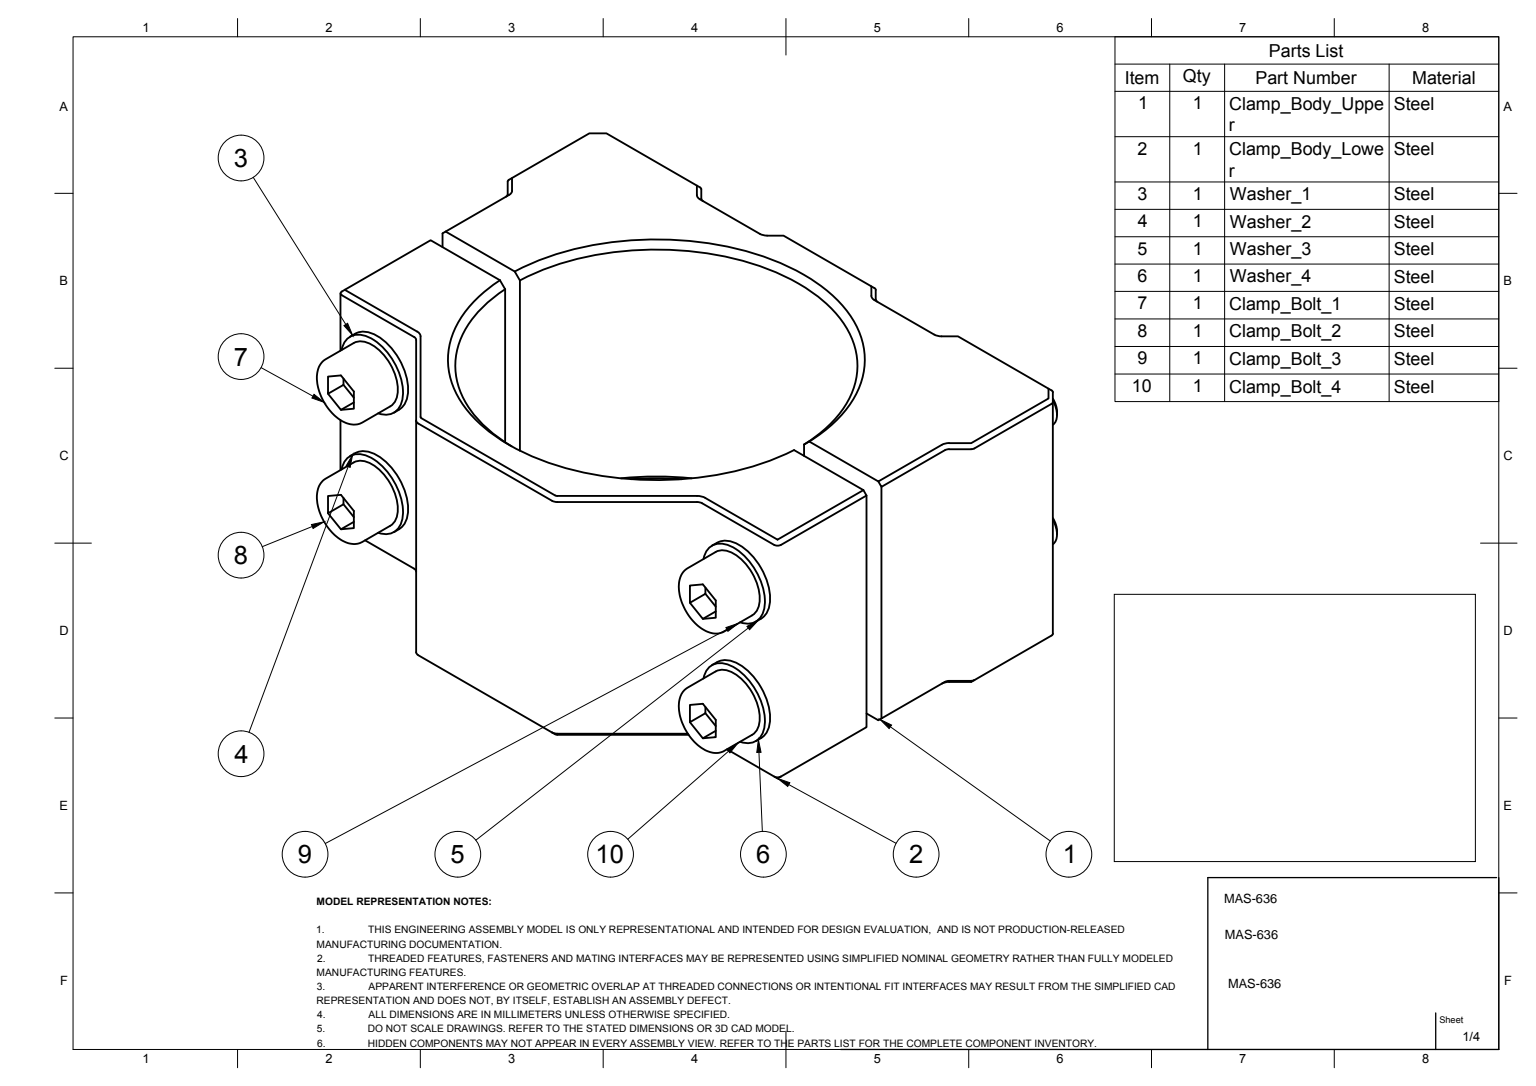
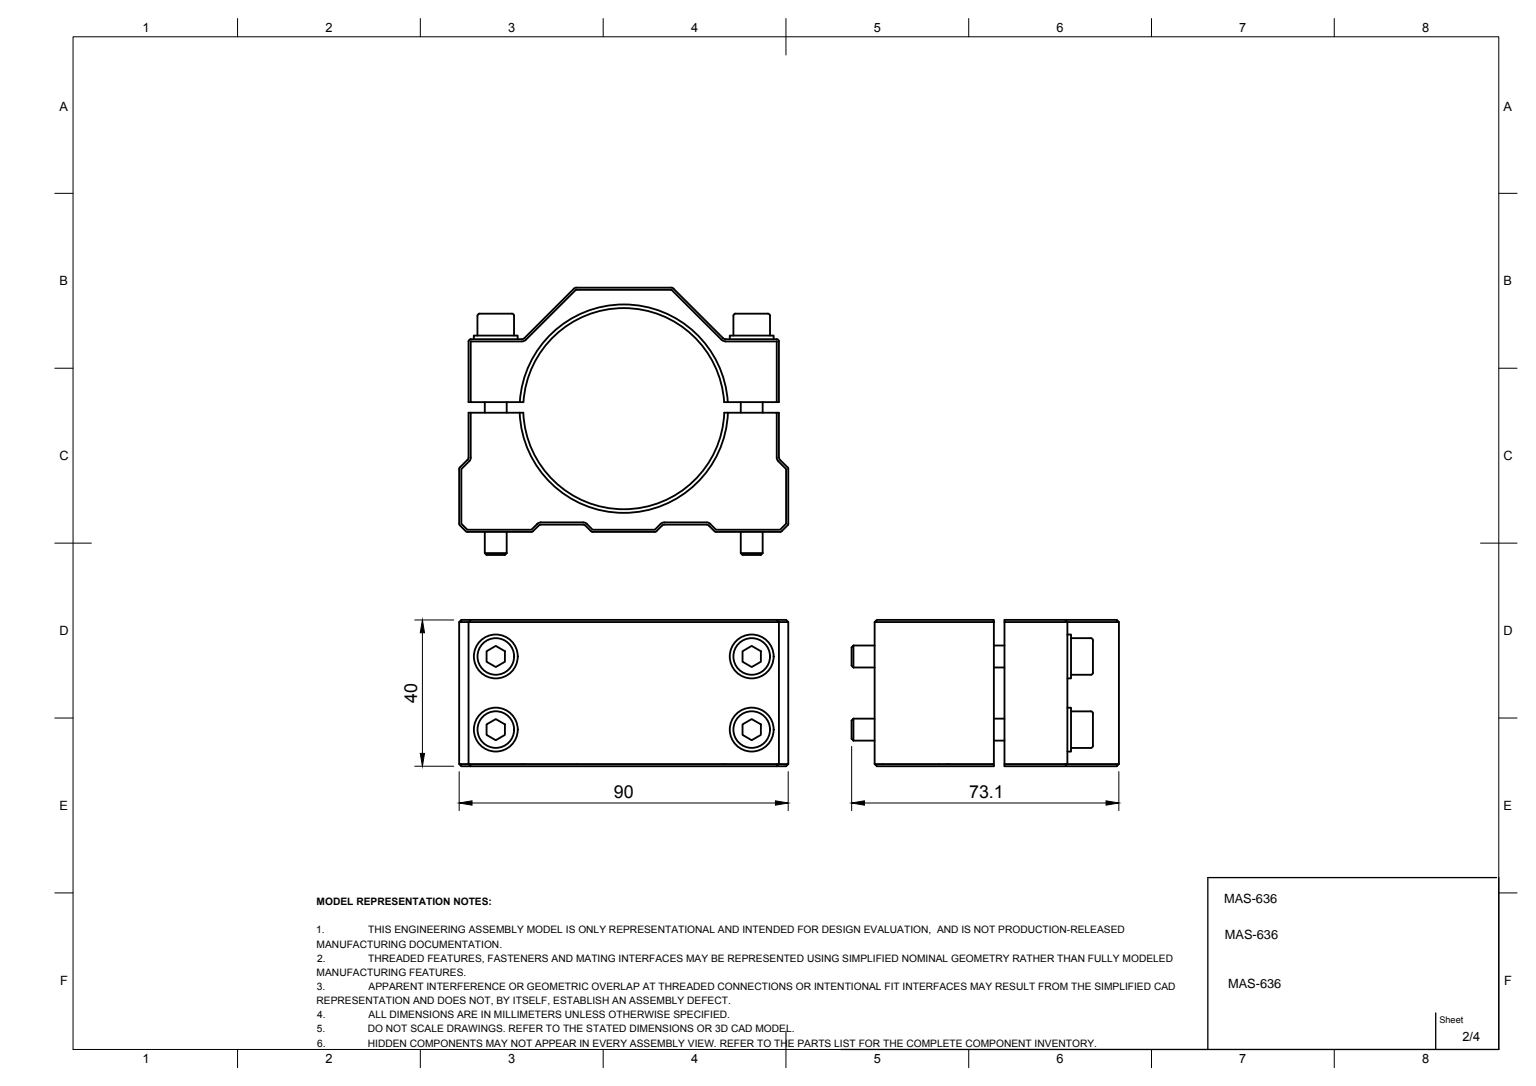
ISO-10303-21;
HEADER;
FILE_DESCRIPTION((''),'2;1');
FILE_NAME('MAS-636','2026-10-09T10:15:02-07:00',(''),(''),'','','');
FILE_SCHEMA (('AUTOMOTIVE_DESIGN { 1 0 10303 214 3 1 1 }'));
ENDSEC;
DATA;
#10 = MECHANICAL_DESIGN_GEOMETRIC_PRESENTATION_REPRESENTATION('',(#83,#84,
#85,#86,#87,#88,#89,#90,#91,#92),#6779) ;
#11 = ITEM_DEFINED_TRANSFORMATION($,$,#4017,#4427) ;
#12 = ITEM_DEFINED_TRANSFORMATION($,$,#4192,#4428) ;
#13 = ITEM_DEFINED_TRANSFORMATION($,$,#4291,#4429) ;
#14 = ITEM_DEFINED_TRANSFORMATION($,$,#4300,#4430) ;
#15 = ITEM_DEFINED_TRANSFORMATION($,$,#4309,#4431) ;
#16 = ITEM_DEFINED_TRANSFORMATION($,$,#4318,#4432) ;
#17 = ITEM_DEFINED_TRANSFORMATION($,$,#4327,#4433) ;
#18 = ITEM_DEFINED_TRANSFORMATION($,$,#4352,#4434) ;
#19 = ITEM_DEFINED_TRANSFORMATION($,$,#4377,#4435) ;
#20 = ITEM_DEFINED_TRANSFORMATION($,$,#4402,#4436) ;
#21 = (
REPRESENTATION_RELATIONSHIP($,$,#6817,#6816)
REPRESENTATION_RELATIONSHIP_WITH_TRANSFORMATION(#11)
SHAPE_REPRESENTATION_RELATIONSHIP()
) ;
#22 = (
REPRESENTATION_RELATIONSHIP($,$,#6818,#6816)
REPRESENTATION_RELATIONSHIP_WITH_TRANSFORMATION(#12)
SHAPE_REPRESENTATION_RELATIONSHIP()
) ;
#23 = (
REPRESENTATION_RELATIONSHIP($,$,#6819,#6816)
REPRESENTATION_RELATIONSHIP_WITH_TRANSFORMATION(#13)
SHAPE_REPRESENTATION_RELATIONSHIP()
) ;
#24 = (
REPRESENTATION_RELATIONSHIP($,$,#6820,#6816)
REPRESENTATION_RELATIONSHIP_WITH_TRANSFORMATION(#14)
SHAPE_REPRESENTATION_RELATIONSHIP()
) ;
#25 = (
REPRESENTATION_RELATIONSHIP($,$,#6821,#6816)
REPRESENTATION_RELATIONSHIP_WITH_TRANSFORMATION(#15)
SHAPE_REPRESENTATION_RELATIONSHIP()
) ;
#26 = (
REPRESENTATION_RELATIONSHIP($,$,#6822,#6816)
REPRESENTATION_RELATIONSHIP_WITH_TRANSFORMATION(#16)
SHAPE_REPRESENTATION_RELATIONSHIP()
) ;
#27 = (
REPRESENTATION_RELATIONSHIP($,$,#6823,#6816)
REPRESENTATION_RELATIONSHIP_WITH_TRANSFORMATION(#17)
SHAPE_REPRESENTATION_RELATIONSHIP()
) ;
#28 = (
REPRESENTATION_RELATIONSHIP($,$,#6824,#6816)
REPRESENTATION_RELATIONSHIP_WITH_TRANSFORMATION(#18)
SHAPE_REPRESENTATION_RELATIONSHIP()
) ;
#29 = (
REPRESENTATION_RELATIONSHIP($,$,#6825,#6816)
REPRESENTATION_RELATIONSHIP_WITH_TRANSFORMATION(#19)
SHAPE_REPRESENTATION_RELATIONSHIP()
) ;
#30 = (
REPRESENTATION_RELATIONSHIP($,$,#6826,#6816)
REPRESENTATION_RELATIONSHIP_WITH_TRANSFORMATION(#20)
SHAPE_REPRESENTATION_RELATIONSHIP()
) ;
#31 = CONTEXT_DEPENDENT_SHAPE_REPRESENTATION(#21,#6806) ;
#32 = CONTEXT_DEPENDENT_SHAPE_REPRESENTATION(#22,#6807) ;
#33 = CONTEXT_DEPENDENT_SHAPE_REPRESENTATION(#23,#6808) ;
#34 = CONTEXT_DEPENDENT_SHAPE_REPRESENTATION(#24,#6809) ;
#35 = CONTEXT_DEPENDENT_SHAPE_REPRESENTATION(#25,#6810) ;
#36 = CONTEXT_DEPENDENT_SHAPE_REPRESENTATION(#26,#6811) ;
#37 = CONTEXT_DEPENDENT_SHAPE_REPRESENTATION(#27,#6812) ;
#38 = CONTEXT_DEPENDENT_SHAPE_REPRESENTATION(#28,#6813) ;
#39 = CONTEXT_DEPENDENT_SHAPE_REPRESENTATION(#29,#6814) ;
#40 = CONTEXT_DEPENDENT_SHAPE_REPRESENTATION(#30,#6815) ;
#41 = NEXT_ASSEMBLY_USAGE_OCCURRENCE('Clamp_Body_Upper:1',
'Clamp_Body_Upper:1','Clamp_Body_Upper:1',#6828,#6829,
'Clamp_Body_Upper:1') ;
#42 = NEXT_ASSEMBLY_USAGE_OCCURRENCE('Clamp_Body_Lower:1',
'Clamp_Body_Lower:1','Clamp_Body_Lower:1',#6828,#6830,
'Clamp_Body_Lower:1') ;
#43 = NEXT_ASSEMBLY_USAGE_OCCURRENCE('Washer_1:1','Washer_1:1',
'Washer_1:1',#6828,#6831,'Washer_1:1') ;
#44 = NEXT_ASSEMBLY_USAGE_OCCURRENCE('Washer_2:1','Washer_2:1',
'Washer_2:1',#6828,#6832,'Washer_2:1') ;
#45 = NEXT_ASSEMBLY_USAGE_OCCURRENCE('Washer_3:1','Washer_3:1',
'Washer_3:1',#6828,#6833,'Washer_3:1') ;
#46 = NEXT_ASSEMBLY_USAGE_OCCURRENCE('Washer_4:1','Washer_4:1',
'Washer_4:1',#6828,#6834,'Washer_4:1') ;
#47 = NEXT_ASSEMBLY_USAGE_OCCURRENCE('Clamp_Bolt_1:1','Clamp_Bolt_1:1',
'Clamp_Bolt_1:1',#6828,#6835,'Clamp_Bolt_1:1') ;
#48 = NEXT_ASSEMBLY_USAGE_OCCURRENCE('Clamp_Bolt_2:1','Clamp_Bolt_2:1',
'Clamp_Bolt_2:1',#6828,#6836,'Clamp_Bolt_2:1') ;
#49 = NEXT_ASSEMBLY_USAGE_OCCURRENCE('Clamp_Bolt_3:1','Clamp_Bolt_3:1',
'Clamp_Bolt_3:1',#6828,#6837,'Clamp_Bolt_3:1') ;
#50 = NEXT_ASSEMBLY_USAGE_OCCURRENCE('Clamp_Bolt_4:1','Clamp_Bolt_4:1',
'Clamp_Bolt_4:1',#6828,#6838,'Clamp_Bolt_4:1') ;
#51 = TOROIDAL_SURFACE('',#4342,4.4,0.6) ;
#52 = TOROIDAL_SURFACE('',#4346,3.25,0.25) ;
#53 = TOROIDAL_SURFACE('',#4367,4.4,0.6) ;
#54 = TOROIDAL_SURFACE('',#4371,3.25,0.25) ;
#55 = TOROIDAL_SURFACE('',#4392,4.4,0.6) ;
#56 = TOROIDAL_SURFACE('',#4396,3.25,0.25) ;
#57 = TOROIDAL_SURFACE('',#4417,4.4,0.6) ;
#58 = TOROIDAL_SURFACE('',#4421,3.25,0.25) ;
#59 = B_SPLINE_CURVE_WITH_KNOTS('',3,(#6151,#6152,#6153,#6154),
 .UNSPECIFIED.,.F.,.F.,(4,4),(0.,2.0142284459),.UNSPECIFIED.) ;
#60 = B_SPLINE_CURVE_WITH_KNOTS('',3,(#6158,#6159,#6160,#6161),
 .UNSPECIFIED.,.F.,.F.,(4,4),(0.,2.0142284459),.UNSPECIFIED.) ;
#61 = B_SPLINE_CURVE_WITH_KNOTS('',3,(#6173,#6174,#6175,#6176),
 .UNSPECIFIED.,.F.,.F.,(4,4),(0.,2.0142284459),.UNSPECIFIED.) ;
#62 = B_SPLINE_CURVE_WITH_KNOTS('',3,(#6177,#6178,#6179,#6180),
 .UNSPECIFIED.,.F.,.F.,(4,4),(0.,2.0142284459),.UNSPECIFIED.) ;
#63 = SHAPE_REPRESENTATION_RELATIONSHIP('SRR','None',#6817,#73) ;
#64 = SHAPE_REPRESENTATION_RELATIONSHIP('SRR','None',#6818,#74) ;
#65 = SHAPE_REPRESENTATION_RELATIONSHIP('SRR','None',#6819,#75) ;
#66 = SHAPE_REPRESENTATION_RELATIONSHIP('SRR','None',#6820,#76) ;
#67 = SHAPE_REPRESENTATION_RELATIONSHIP('SRR','None',#6821,#77) ;
#68 = SHAPE_REPRESENTATION_RELATIONSHIP('SRR','None',#6822,#78) ;
#69 = SHAPE_REPRESENTATION_RELATIONSHIP('SRR','None',#6823,#79) ;
#70 = SHAPE_REPRESENTATION_RELATIONSHIP('SRR','None',#6824,#80) ;
#71 = SHAPE_REPRESENTATION_RELATIONSHIP('SRR','None',#6825,#81) ;
#72 = SHAPE_REPRESENTATION_RELATIONSHIP('SRR','None',#6826,#82) ;
#73 = ADVANCED_BREP_SHAPE_REPRESENTATION('',(#93),#6769) ;
#74 = ADVANCED_BREP_SHAPE_REPRESENTATION('',(#94),#6770) ;
#75 = ADVANCED_BREP_SHAPE_REPRESENTATION('',(#95),#6771) ;
#76 = ADVANCED_BREP_SHAPE_REPRESENTATION('',(#96),#6772) ;
#77 = ADVANCED_BREP_SHAPE_REPRESENTATION('',(#97),#6773) ;
#78 = ADVANCED_BREP_SHAPE_REPRESENTATION('',(#98),#6774) ;
#79 = ADVANCED_BREP_SHAPE_REPRESENTATION('',(#99),#6775) ;
#80 = ADVANCED_BREP_SHAPE_REPRESENTATION('',(#100),#6776) ;
#81 = ADVANCED_BREP_SHAPE_REPRESENTATION('',(#101),#6777) ;
#82 = ADVANCED_BREP_SHAPE_REPRESENTATION('',(#102),#6778) ;
#83 = STYLED_ITEM('',(#6876),#93) ;
#84 = STYLED_ITEM('',(#6876),#94) ;
#85 = STYLED_ITEM('',(#6877),#95) ;
#86 = STYLED_ITEM('',(#6877),#96) ;
#87 = STYLED_ITEM('',(#6877),#97) ;
#88 = STYLED_ITEM('',(#6877),#98) ;
#89 = STYLED_ITEM('',(#6877),#99) ;
#90 = STYLED_ITEM('',(#6877),#100) ;
#91 = STYLED_ITEM('',(#6877),#101) ;
#92 = STYLED_ITEM('',(#6877),#102) ;
#93 = MANIFOLD_SOLID_BREP('Body1',#3895) ;
#94 = MANIFOLD_SOLID_BREP('Body1',#3896) ;
#95 = MANIFOLD_SOLID_BREP('Body1',#3897) ;
#96 = MANIFOLD_SOLID_BREP('Body1',#3898) ;
#97 = MANIFOLD_SOLID_BREP('Body1',#3899) ;
#98 = MANIFOLD_SOLID_BREP('Body1',#3900) ;
#99 = MANIFOLD_SOLID_BREP('Body1',#3901) ;
#100 = MANIFOLD_SOLID_BREP('Body1',#3902) ;
#101 = MANIFOLD_SOLID_BREP('Body1',#3903) ;
#102 = MANIFOLD_SOLID_BREP('Body1',#3904) ;
#103 = FACE_BOUND('',#628,.T.) ;
#104 = FACE_BOUND('',#629,.T.) ;
#105 = FACE_BOUND('',#631,.T.) ;
#106 = FACE_BOUND('',#632,.T.) ;
#107 = FACE_BOUND('',#638,.T.) ;
#108 = FACE_BOUND('',#639,.T.) ;
#109 = FACE_BOUND('',#649,.T.) ;
#110 = FACE_BOUND('',#650,.T.) ;
#111 = FACE_BOUND('',#719,.T.) ;
#112 = FACE_BOUND('',#720,.T.) ;
#113 = FACE_BOUND('',#722,.T.) ;
#114 = FACE_BOUND('',#723,.T.) ;
#115 = FACE_BOUND('',#745,.T.) ;
#116 = FACE_BOUND('',#746,.T.) ;
#117 = FACE_BOUND('',#752,.T.) ;
#118 = FACE_BOUND('',#753,.T.) ;
#119 = FACE_BOUND('',#758,.T.) ;
#120 = FACE_BOUND('',#760,.T.) ;
#121 = FACE_BOUND('',#764,.T.) ;
#122 = FACE_BOUND('',#766,.T.) ;
#123 = FACE_BOUND('',#770,.T.) ;
#124 = FACE_BOUND('',#772,.T.) ;
#125 = FACE_BOUND('',#776,.T.) ;
#126 = FACE_BOUND('',#778,.T.) ;
#127 = FACE_BOUND('',#787,.T.) ;
#128 = FACE_BOUND('',#789,.T.) ;
#129 = FACE_BOUND('',#804,.T.) ;
#130 = FACE_BOUND('',#806,.T.) ;
#131 = FACE_BOUND('',#821,.T.) ;
#132 = FACE_BOUND('',#823,.T.) ;
#133 = FACE_BOUND('',#838,.T.) ;
#134 = FACE_BOUND('',#840,.T.) ;
#135 = PLANE('',#4045) ;
#136 = PLANE('',#4054) ;
#137 = PLANE('',#4057) ;
#138 = PLANE('',#4060) ;
#139 = PLANE('',#4063) ;
#140 = PLANE('',#4066) ;
#141 = PLANE('',#4069) ;
#142 = PLANE('',#4072) ;
#143 = PLANE('',#4075) ;
#144 = PLANE('',#4078) ;
#145 = PLANE('',#4081) ;
#146 = PLANE('',#4084) ;
#147 = PLANE('',#4087) ;
#148 = PLANE('',#4090) ;
#149 = PLANE('',#4093) ;
#150 = PLANE('',#4096) ;
#151 = PLANE('',#4099) ;
#152 = PLANE('',#4100) ;
#153 = PLANE('',#4101) ;
#154 = PLANE('',#4120) ;
#155 = PLANE('',#4121) ;
#156 = PLANE('',#4122) ;
#157 = PLANE('',#4123) ;
#158 = PLANE('',#4124) ;
#159 = PLANE('',#4125) ;
#160 = PLANE('',#4128) ;
#161 = PLANE('',#4131) ;
#162 = PLANE('',#4132) ;
#163 = PLANE('',#4135) ;
#164 = PLANE('',#4138) ;
#165 = PLANE('',#4139) ;
#166 = PLANE('',#4142) ;
#167 = PLANE('',#4145) ;
#168 = PLANE('',#4148) ;
#169 = PLANE('',#4151) ;
#170 = PLANE('',#4152) ;
#171 = PLANE('',#4155) ;
#172 = PLANE('',#4156) ;
#173 = PLANE('',#4160) ;
#174 = PLANE('',#4162) ;
#175 = PLANE('',#4164) ;
#176 = PLANE('',#4166) ;
#177 = PLANE('',#4168) ;
#178 = PLANE('',#4170) ;
#179 = PLANE('',#4172) ;
#180 = PLANE('',#4174) ;
#181 = PLANE('',#4176) ;
#182 = PLANE('',#4178) ;
#183 = PLANE('',#4180) ;
#184 = PLANE('',#4182) ;
#185 = PLANE('',#4184) ;
#186 = PLANE('',#4186) ;
#187 = PLANE('',#4188) ;
#188 = PLANE('',#4190) ;
#189 = PLANE('',#4191) ;
#190 = PLANE('',#4200) ;
#191 = PLANE('',#4209) ;
#192 = PLANE('',#4212) ;
#193 = PLANE('',#4215) ;
#194 = PLANE('',#4218) ;
#195 = PLANE('',#4221) ;
#196 = PLANE('',#4224) ;
#197 = PLANE('',#4225) ;
#198 = PLANE('',#4226) ;
#199 = PLANE('',#4237) ;
#200 = PLANE('',#4238) ;
#201 = PLANE('',#4241) ;
#202 = PLANE('',#4244) ;
#203 = PLANE('',#4247) ;
#204 = PLANE('',#4250) ;
#205 = PLANE('',#4253) ;
#206 = PLANE('',#4257) ;
#207 = PLANE('',#4259) ;
#208 = PLANE('',#4261) ;
#209 = PLANE('',#4263) ;
#210 = PLANE('',#4265) ;
#211 = PLANE('',#4267) ;
#212 = PLANE('',#4268) ;
#213 = PLANE('',#4277) ;
#214 = PLANE('',#4288) ;
#215 = PLANE('',#4298) ;
#216 = PLANE('',#4299) ;
#217 = PLANE('',#4307) ;
#218 = PLANE('',#4308) ;
#219 = PLANE('',#4316) ;
#220 = PLANE('',#4317) ;
#221 = PLANE('',#4325) ;
#222 = PLANE('',#4326) ;
#223 = PLANE('',#4328) ;
#224 = PLANE('',#4329) ;
#225 = PLANE('',#4330) ;
#226 = PLANE('',#4331) ;
#227 = PLANE('',#4332) ;
#228 = PLANE('',#4333) ;
#229 = PLANE('',#4334) ;
#230 = PLANE('',#4335) ;
#231 = PLANE('',#4337) ;
#232 = PLANE('',#4340) ;
#233 = PLANE('',#4353) ;
#234 = PLANE('',#4354) ;
#235 = PLANE('',#4355) ;
#236 = PLANE('',#4356) ;
#237 = PLANE('',#4357) ;
#238 = PLANE('',#4358) ;
#239 = PLANE('',#4359) ;
#240 = PLANE('',#4360) ;
#241 = PLANE('',#4362) ;
#242 = PLANE('',#4365) ;
#243 = PLANE('',#4378) ;
#244 = PLANE('',#4379) ;
#245 = PLANE('',#4380) ;
#246 = PLANE('',#4381) ;
#247 = PLANE('',#4382) ;
#248 = PLANE('',#4383) ;
#249 = PLANE('',#4384) ;
#250 = PLANE('',#4385) ;
#251 = PLANE('',#4387) ;
#252 = PLANE('',#4390) ;
#253 = PLANE('',#4403) ;
#254 = PLANE('',#4404) ;
#255 = PLANE('',#4405) ;
#256 = PLANE('',#4406) ;
#257 = PLANE('',#4407) ;
#258 = PLANE('',#4408) ;
#259 = PLANE('',#4409) ;
#260 = PLANE('',#4410) ;
#261 = PLANE('',#4412) ;
#262 = PLANE('',#4415) ;
#263 = (
BOUNDED_CURVE()
B_SPLINE_CURVE(2,(#5652,#5653,#5654),.UNSPECIFIED.,.F.,.F.)
B_SPLINE_CURVE_WITH_KNOTS((3,3),(8.17571637705571,8.18145882895963),
 .UNSPECIFIED.)
CURVE()
GEOMETRIC_REPRESENTATION_ITEM()
RATIONAL_B_SPLINE_CURVE((1.06993006993377,1.0518696293833,1.03378378378363))
REPRESENTATION_ITEM('')
) ;
#264 = (
BOUNDED_CURVE()
B_SPLINE_CURVE(2,(#5656,#5657,#5658),.UNSPECIFIED.,.F.,.F.)
B_SPLINE_CURVE_WITH_KNOTS((3,3),(-0.0111022969227764,-0.00535984501964869),
 .UNSPECIFIED.)
CURVE()
GEOMETRIC_REPRESENTATION_ITEM()
RATIONAL_B_SPLINE_CURVE((1.06993006993377,1.0518696293858,1.03378378378863))
REPRESENTATION_ITEM('')
) ;
#265 = (
BOUNDED_CURVE()
B_SPLINE_CURVE(2,(#5664,#5665,#5666),.UNSPECIFIED.,.F.,.F.)
B_SPLINE_CURVE_WITH_KNOTS((3,3),(8.1757163770557,8.18145882895962),
 .UNSPECIFIED.)
CURVE()
GEOMETRIC_REPRESENTATION_ITEM()
RATIONAL_B_SPLINE_CURVE((1.06993006993376,1.05186962938329,1.03378378378362))
REPRESENTATION_ITEM('')
) ;
#266 = (
BOUNDED_CURVE()
B_SPLINE_CURVE(2,(#5667,#5668,#5669),.UNSPECIFIED.,.F.,.F.)
B_SPLINE_CURVE_WITH_KNOTS((3,3),(-0.0111022969227769,-0.00535984501964911),
 .UNSPECIFIED.)
CURVE()
GEOMETRIC_REPRESENTATION_ITEM()
RATIONAL_B_SPLINE_CURVE((1.06993006993377,1.0518696293858,1.03378378378863))
REPRESENTATION_ITEM('')
) ;
#267 = CONICAL_SURFACE('',#4021,1.,0.785398163397) ;
#268 = CONICAL_SURFACE('',#4023,1.,0.785398163397) ;
#269 = CONICAL_SURFACE('',#4028,1.,0.785398163398) ;
#270 = CONICAL_SURFACE('',#4033,1.,0.785398163398) ;
#271 = CONICAL_SURFACE('',#4038,1.,0.785398163398) ;
#272 = CONICAL_SURFACE('',#4043,1.,0.785398163398) ;
#273 = CONICAL_SURFACE('',#4052,1.,0.785398163392) ;
#274 = CONICAL_SURFACE('',#4055,1.,0.785398163397) ;
#275 = CONICAL_SURFACE('',#4058,1.,0.785398163397) ;
#276 = CONICAL_SURFACE('',#4061,1.,0.785398163397) ;
#277 = CONICAL_SURFACE('',#4064,1.,0.785398163397) ;
#278 = CONICAL_SURFACE('',#4067,1.,0.785398163392) ;
#279 = CONICAL_SURFACE('',#4070,1.,0.785398163392) ;
#280 = CONICAL_SURFACE('',#4073,1.,0.785398163397) ;
#281 = CONICAL_SURFACE('',#4076,1.,0.785398163397) ;
#282 = CONICAL_SURFACE('',#4079,1.,0.785398163397) ;
#283 = CONICAL_SURFACE('',#4082,1.,0.785398163397) ;
#284 = CONICAL_SURFACE('',#4085,1.,0.785398163397) ;
#285 = CONICAL_SURFACE('',#4088,1.,0.785398163397) ;
#286 = CONICAL_SURFACE('',#4091,1.,0.785398163397) ;
#287 = CONICAL_SURFACE('',#4094,1.,0.785398163397) ;
#288 = CONICAL_SURFACE('',#4097,1.,0.785398163397) ;
#289 = CONICAL_SURFACE('',#4159,1.,0.785398163392) ;
#290 = CONICAL_SURFACE('',#4161,1.,0.785398163397) ;
#291 = CONICAL_SURFACE('',#4163,1.,0.785398163397) ;
#292 = CONICAL_SURFACE('',#4165,1.,0.785398163397) ;
#293 = CONICAL_SURFACE('',#4167,1.,0.785398163397) ;
#294 = CONICAL_SURFACE('',#4169,1.,0.785398163372) ;
#295 = CONICAL_SURFACE('',#4171,1.,0.785398163372) ;
#296 = CONICAL_SURFACE('',#4173,1.,0.785398163397) ;
#297 = CONICAL_SURFACE('',#4175,1.,0.785398163397) ;
#298 = CONICAL_SURFACE('',#4177,1.,0.785398163397) ;
#299 = CONICAL_SURFACE('',#4179,1.,0.785398163397) ;
#300 = CONICAL_SURFACE('',#4181,1.,0.785398163397) ;
#301 = CONICAL_SURFACE('',#4183,1.,0.785398163397) ;
#302 = CONICAL_SURFACE('',#4185,1.,0.785398163397) ;
#303 = CONICAL_SURFACE('',#4187,1.,0.785398163397) ;
#304 = CONICAL_SURFACE('',#4189,1.,0.785398163397) ;
#305 = CONICAL_SURFACE('',#4193,1.,0.785398163397) ;
#306 = CONICAL_SURFACE('',#4198,1.,0.785398163397) ;
#307 = CONICAL_SURFACE('',#4207,1.,0.785398163397) ;
#308 = CONICAL_SURFACE('',#4210,1.,0.785398163397) ;
#309 = CONICAL_SURFACE('',#4213,1.,0.785398163397) ;
#310 = CONICAL_SURFACE('',#4216,1.,0.785398163397) ;
#311 = CONICAL_SURFACE('',#4219,1.,0.785398163397) ;
#312 = CONICAL_SURFACE('',#4222,1.,0.785398163397) ;
#313 = CONICAL_SURFACE('',#4256,1.,0.785398163397) ;
#314 = CONICAL_SURFACE('',#4258,1.,0.785398163397) ;
#315 = CONICAL_SURFACE('',#4260,1.,0.785398163397) ;
#316 = CONICAL_SURFACE('',#4262,1.,0.785398163397) ;
#317 = CONICAL_SURFACE('',#4264,1.,0.785398163397) ;
#318 = CONICAL_SURFACE('',#4266,1.,0.785398163397) ;
#319 = CONICAL_SURFACE('',#4272,1.,0.785398163398) ;
#320 = CONICAL_SURFACE('',#4279,1.,0.785398163398) ;
#321 = CONICAL_SURFACE('',#4283,1.,0.785398163398) ;
#322 = CONICAL_SURFACE('',#4290,1.,0.785398163398) ;
#323 = CONICAL_SURFACE('',#4351,2.5,0.785398163397) ;
#324 = CONICAL_SURFACE('',#4376,2.5,0.785398163397) ;
#325 = CONICAL_SURFACE('',#4401,2.5,0.785398163397) ;
#326 = CONICAL_SURFACE('',#4426,2.5,0.785398163397) ;
#327 = FACE_OUTER_BOUND('',#571,.T.) ;
#328 = FACE_OUTER_BOUND('',#572,.T.) ;
#329 = FACE_OUTER_BOUND('',#573,.T.) ;
#330 = FACE_OUTER_BOUND('',#574,.T.) ;
#331 = FACE_OUTER_BOUND('',#575,.T.) ;
#332 = FACE_OUTER_BOUND('',#576,.T.) ;
#333 = FACE_OUTER_BOUND('',#577,.T.) ;
#334 = FACE_OUTER_BOUND('',#578,.T.) ;
#335 = FACE_OUTER_BOUND('',#579,.T.) ;
#336 = FACE_OUTER_BOUND('',#580,.T.) ;
#337 = FACE_OUTER_BOUND('',#581,.T.) ;
#338 = FACE_OUTER_BOUND('',#582,.T.) ;
#339 = FACE_OUTER_BOUND('',#583,.T.) ;
#340 = FACE_OUTER_BOUND('',#584,.T.) ;
#341 = FACE_OUTER_BOUND('',#585,.T.) ;
#342 = FACE_OUTER_BOUND('',#586,.T.) ;
#343 = FACE_OUTER_BOUND('',#587,.T.) ;
#344 = FACE_OUTER_BOUND('',#588,.T.) ;
#345 = FACE_OUTER_BOUND('',#589,.T.) ;
#346 = FACE_OUTER_BOUND('',#590,.T.) ;
#347 = FACE_OUTER_BOUND('',#591,.T.) ;
#348 = FACE_OUTER_BOUND('',#592,.T.) ;
#349 = FACE_OUTER_BOUND('',#593,.T.) ;
#350 = FACE_OUTER_BOUND('',#594,.T.) ;
#351 = FACE_OUTER_BOUND('',#595,.T.) ;
#352 = FACE_OUTER_BOUND('',#596,.T.) ;
#353 = FACE_OUTER_BOUND('',#597,.T.) ;
#354 = FACE_OUTER_BOUND('',#598,.T.) ;
#355 = FACE_OUTER_BOUND('',#599,.T.) ;
#356 = FACE_OUTER_BOUND('',#600,.T.) ;
#357 = FACE_OUTER_BOUND('',#601,.T.) ;
#358 = FACE_OUTER_BOUND('',#602,.T.) ;
#359 = FACE_OUTER_BOUND('',#603,.T.) ;
#360 = FACE_OUTER_BOUND('',#604,.T.) ;
#361 = FACE_OUTER_BOUND('',#605,.T.) ;
#362 = FACE_OUTER_BOUND('',#606,.T.) ;
#363 = FACE_OUTER_BOUND('',#607,.T.) ;
#364 = FACE_OUTER_BOUND('',#608,.T.) ;
#365 = FACE_OUTER_BOUND('',#609,.T.) ;
#366 = FACE_OUTER_BOUND('',#610,.T.) ;
#367 = FACE_OUTER_BOUND('',#611,.T.) ;
#368 = FACE_OUTER_BOUND('',#612,.T.) ;
#369 = FACE_OUTER_BOUND('',#613,.T.) ;
#370 = FACE_OUTER_BOUND('',#614,.T.) ;
#371 = FACE_OUTER_BOUND('',#615,.T.) ;
#372 = FACE_OUTER_BOUND('',#616,.T.) ;
#373 = FACE_OUTER_BOUND('',#617,.T.) ;
#374 = FACE_OUTER_BOUND('',#618,.T.) ;
#375 = FACE_OUTER_BOUND('',#619,.T.) ;
#376 = FACE_OUTER_BOUND('',#620,.T.) ;
#377 = FACE_OUTER_BOUND('',#621,.T.) ;
#378 = FACE_OUTER_BOUND('',#622,.T.) ;
#379 = FACE_OUTER_BOUND('',#623,.T.) ;
#380 = FACE_OUTER_BOUND('',#624,.T.) ;
#381 = FACE_OUTER_BOUND('',#625,.T.) ;
#382 = FACE_OUTER_BOUND('',#626,.T.) ;
#383 = FACE_OUTER_BOUND('',#627,.T.) ;
#384 = FACE_OUTER_BOUND('',#630,.T.) ;
#385 = FACE_OUTER_BOUND('',#633,.T.) ;
#386 = FACE_OUTER_BOUND('',#634,.T.) ;
#387 = FACE_OUTER_BOUND('',#635,.T.) ;
#388 = FACE_OUTER_BOUND('',#636,.T.) ;
#389 = FACE_OUTER_BOUND('',#637,.T.) ;
#390 = FACE_OUTER_BOUND('',#640,.T.) ;
#391 = FACE_OUTER_BOUND('',#641,.T.) ;
#392 = FACE_OUTER_BOUND('',#642,.T.) ;
#393 = FACE_OUTER_BOUND('',#643,.T.) ;
#394 = FACE_OUTER_BOUND('',#644,.T.) ;
#395 = FACE_OUTER_BOUND('',#645,.T.) ;
#396 = FACE_OUTER_BOUND('',#646,.T.) ;
#397 = FACE_OUTER_BOUND('',#647,.T.) ;
#398 = FACE_OUTER_BOUND('',#648,.T.) ;
#399 = FACE_OUTER_BOUND('',#651,.T.) ;
#400 = FACE_OUTER_BOUND('',#652,.T.) ;
#401 = FACE_OUTER_BOUND('',#653,.T.) ;
#402 = FACE_OUTER_BOUND('',#654,.T.) ;
#403 = FACE_OUTER_BOUND('',#655,.T.) ;
#404 = FACE_OUTER_BOUND('',#656,.T.) ;
#405 = FACE_OUTER_BOUND('',#657,.T.) ;
#406 = FACE_OUTER_BOUND('',#658,.T.) ;
#407 = FACE_OUTER_BOUND('',#659,.T.) ;
#408 = FACE_OUTER_BOUND('',#660,.T.) ;
#409 = FACE_OUTER_BOUND('',#661,.T.) ;
#410 = FACE_OUTER_BOUND('',#662,.T.) ;
#411 = FACE_OUTER_BOUND('',#663,.T.) ;
#412 = FACE_OUTER_BOUND('',#664,.T.) ;
#413 = FACE_OUTER_BOUND('',#665,.T.) ;
#414 = FACE_OUTER_BOUND('',#666,.T.) ;
#415 = FACE_OUTER_BOUND('',#667,.T.) ;
#416 = FACE_OUTER_BOUND('',#668,.T.) ;
#417 = FACE_OUTER_BOUND('',#669,.T.) ;
#418 = FACE_OUTER_BOUND('',#670,.T.) ;
#419 = FACE_OUTER_BOUND('',#671,.T.) ;
#420 = FACE_OUTER_BOUND('',#672,.T.) ;
#421 = FACE_OUTER_BOUND('',#673,.T.) ;
#422 = FACE_OUTER_BOUND('',#674,.T.) ;
#423 = FACE_OUTER_BOUND('',#675,.T.) ;
#424 = FACE_OUTER_BOUND('',#676,.T.) ;
#425 = FACE_OUTER_BOUND('',#677,.T.) ;
#426 = FACE_OUTER_BOUND('',#678,.T.) ;
#427 = FACE_OUTER_BOUND('',#679,.T.) ;
#428 = FACE_OUTER_BOUND('',#680,.T.) ;
#429 = FACE_OUTER_BOUND('',#681,.T.) ;
#430 = FACE_OUTER_BOUND('',#682,.T.) ;
#431 = FACE_OUTER_BOUND('',#683,.T.) ;
#432 = FACE_OUTER_BOUND('',#684,.T.) ;
#433 = FACE_OUTER_BOUND('',#685,.T.) ;
#434 = FACE_OUTER_BOUND('',#686,.T.) ;
#435 = FACE_OUTER_BOUND('',#687,.T.) ;
#436 = FACE_OUTER_BOUND('',#688,.T.) ;
#437 = FACE_OUTER_BOUND('',#689,.T.) ;
#438 = FACE_OUTER_BOUND('',#690,.T.) ;
#439 = FACE_OUTER_BOUND('',#691,.T.) ;
#440 = FACE_OUTER_BOUND('',#692,.T.) ;
#441 = FACE_OUTER_BOUND('',#693,.T.) ;
#442 = FACE_OUTER_BOUND('',#694,.T.) ;
#443 = FACE_OUTER_BOUND('',#695,.T.) ;
#444 = FACE_OUTER_BOUND('',#696,.T.) ;
#445 = FACE_OUTER_BOUND('',#697,.T.) ;
#446 = FACE_OUTER_BOUND('',#698,.T.) ;
#447 = FACE_OUTER_BOUND('',#699,.T.) ;
#448 = FACE_OUTER_BOUND('',#700,.T.) ;
#449 = FACE_OUTER_BOUND('',#701,.T.) ;
#450 = FACE_OUTER_BOUND('',#702,.T.) ;
#451 = FACE_OUTER_BOUND('',#703,.T.) ;
#452 = FACE_OUTER_BOUND('',#704,.T.) ;
#453 = FACE_OUTER_BOUND('',#705,.T.) ;
#454 = FACE_OUTER_BOUND('',#706,.T.) ;
#455 = FACE_OUTER_BOUND('',#707,.T.) ;
#456 = FACE_OUTER_BOUND('',#708,.T.) ;
#457 = FACE_OUTER_BOUND('',#709,.T.) ;
#458 = FACE_OUTER_BOUND('',#710,.T.) ;
#459 = FACE_OUTER_BOUND('',#711,.T.) ;
#460 = FACE_OUTER_BOUND('',#712,.T.) ;
#461 = FACE_OUTER_BOUND('',#713,.T.) ;
#462 = FACE_OUTER_BOUND('',#714,.T.) ;
#463 = FACE_OUTER_BOUND('',#715,.T.) ;
#464 = FACE_OUTER_BOUND('',#716,.T.) ;
#465 = FACE_OUTER_BOUND('',#717,.T.) ;
#466 = FACE_OUTER_BOUND('',#718,.T.) ;
#467 = FACE_OUTER_BOUND('',#721,.T.) ;
#468 = FACE_OUTER_BOUND('',#724,.T.) ;
#469 = FACE_OUTER_BOUND('',#725,.T.) ;
#470 = FACE_OUTER_BOUND('',#726,.T.) ;
#471 = FACE_OUTER_BOUND('',#727,.T.) ;
#472 = FACE_OUTER_BOUND('',#728,.T.) ;
#473 = FACE_OUTER_BOUND('',#729,.T.) ;
#474 = FACE_OUTER_BOUND('',#730,.T.) ;
#475 = FACE_OUTER_BOUND('',#731,.T.) ;
#476 = FACE_OUTER_BOUND('',#732,.T.) ;
#477 = FACE_OUTER_BOUND('',#733,.T.) ;
#478 = FACE_OUTER_BOUND('',#734,.T.) ;
#479 = FACE_OUTER_BOUND('',#735,.T.) ;
#480 = FACE_OUTER_BOUND('',#736,.T.) ;
#481 = FACE_OUTER_BOUND('',#737,.T.) ;
#482 = FACE_OUTER_BOUND('',#738,.T.) ;
#483 = FACE_OUTER_BOUND('',#739,.T.) ;
#484 = FACE_OUTER_BOUND('',#740,.T.) ;
#485 = FACE_OUTER_BOUND('',#741,.T.) ;
#486 = FACE_OUTER_BOUND('',#742,.T.) ;
#487 = FACE_OUTER_BOUND('',#743,.T.) ;
#488 = FACE_OUTER_BOUND('',#744,.T.) ;
#489 = FACE_OUTER_BOUND('',#747,.T.) ;
#490 = FACE_OUTER_BOUND('',#748,.T.) ;
#491 = FACE_OUTER_BOUND('',#749,.T.) ;
#492 = FACE_OUTER_BOUND('',#750,.T.) ;
#493 = FACE_OUTER_BOUND('',#751,.T.) ;
#494 = FACE_OUTER_BOUND('',#754,.T.) ;
#495 = FACE_OUTER_BOUND('',#755,.T.) ;
#496 = FACE_OUTER_BOUND('',#756,.T.) ;
#497 = FACE_OUTER_BOUND('',#757,.T.) ;
#498 = FACE_OUTER_BOUND('',#759,.T.) ;
#499 = FACE_OUTER_BOUND('',#761,.T.) ;
#500 = FACE_OUTER_BOUND('',#762,.T.) ;
#501 = FACE_OUTER_BOUND('',#763,.T.) ;
#502 = FACE_OUTER_BOUND('',#765,.T.) ;
#503 = FACE_OUTER_BOUND('',#767,.T.) ;
#504 = FACE_OUTER_BOUND('',#768,.T.) ;
#505 = FACE_OUTER_BOUND('',#769,.T.) ;
#506 = FACE_OUTER_BOUND('',#771,.T.) ;
#507 = FACE_OUTER_BOUND('',#773,.T.) ;
#508 = FACE_OUTER_BOUND('',#774,.T.) ;
#509 = FACE_OUTER_BOUND('',#775,.T.) ;
#510 = FACE_OUTER_BOUND('',#777,.T.) ;
#511 = FACE_OUTER_BOUND('',#779,.T.) ;
#512 = FACE_OUTER_BOUND('',#780,.T.) ;
#513 = FACE_OUTER_BOUND('',#781,.T.) ;
#514 = FACE_OUTER_BOUND('',#782,.T.) ;
#515 = FACE_OUTER_BOUND('',#783,.T.) ;
#516 = FACE_OUTER_BOUND('',#784,.T.) ;
#517 = FACE_OUTER_BOUND('',#785,.T.) ;
#518 = FACE_OUTER_BOUND('',#786,.T.) ;
#519 = FACE_OUTER_BOUND('',#788,.T.) ;
#520 = FACE_OUTER_BOUND('',#790,.T.) ;
#521 = FACE_OUTER_BOUND('',#791,.T.) ;
#522 = FACE_OUTER_BOUND('',#792,.T.) ;
#523 = FACE_OUTER_BOUND('',#793,.T.) ;
#524 = FACE_OUTER_BOUND('',#794,.T.) ;
#525 = FACE_OUTER_BOUND('',#795,.T.) ;
#526 = FACE_OUTER_BOUND('',#796,.T.) ;
#527 = FACE_OUTER_BOUND('',#797,.T.) ;
#528 = FACE_OUTER_BOUND('',#798,.T.) ;
#529 = FACE_OUTER_BOUND('',#799,.T.) ;
#530 = FACE_OUTER_BOUND('',#800,.T.) ;
#531 = FACE_OUTER_BOUND('',#801,.T.) ;
#532 = FACE_OUTER_BOUND('',#802,.T.) ;
#533 = FACE_OUTER_BOUND('',#803,.T.) ;
#534 = FACE_OUTER_BOUND('',#805,.T.) ;
#535 = FACE_OUTER_BOUND('',#807,.T.) ;
#536 = FACE_OUTER_BOUND('',#808,.T.) ;
#537 = FACE_OUTER_BOUND('',#809,.T.) ;
#538 = FACE_OUTER_BOUND('',#810,.T.) ;
#539 = FACE_OUTER_BOUND('',#811,.T.) ;
#540 = FACE_OUTER_BOUND('',#812,.T.) ;
#541 = FACE_OUTER_BOUND('',#813,.T.) ;
#542 = FACE_OUTER_BOUND('',#814,.T.) ;
#543 = FACE_OUTER_BOUND('',#815,.T.) ;
#544 = FACE_OUTER_BOUND('',#816,.T.) ;
#545 = FACE_OUTER_BOUND('',#817,.T.) ;
#546 = FACE_OUTER_BOUND('',#818,.T.) ;
#547 = FACE_OUTER_BOUND('',#819,.T.) ;
#548 = FACE_OUTER_BOUND('',#820,.T.) ;
#549 = FACE_OUTER_BOUND('',#822,.T.) ;
#550 = FACE_OUTER_BOUND('',#824,.T.) ;
#551 = FACE_OUTER_BOUND('',#825,.T.) ;
#552 = FACE_OUTER_BOUND('',#826,.T.) ;
#553 = FACE_OUTER_BOUND('',#827,.T.) ;
#554 = FACE_OUTER_BOUND('',#828,.T.) ;
#555 = FACE_OUTER_BOUND('',#829,.T.) ;
#556 = FACE_OUTER_BOUND('',#830,.T.) ;
#557 = FACE_OUTER_BOUND('',#831,.T.) ;
#558 = FACE_OUTER_BOUND('',#832,.T.) ;
#559 = FACE_OUTER_BOUND('',#833,.T.) ;
#560 = FACE_OUTER_BOUND('',#834,.T.) ;
#561 = FACE_OUTER_BOUND('',#835,.T.) ;
#562 = FACE_OUTER_BOUND('',#836,.T.) ;
#563 = FACE_OUTER_BOUND('',#837,.T.) ;
#564 = FACE_OUTER_BOUND('',#839,.T.) ;
#565 = FACE_OUTER_BOUND('',#841,.T.) ;
#566 = FACE_OUTER_BOUND('',#842,.T.) ;
#567 = FACE_OUTER_BOUND('',#843,.T.) ;
#568 = FACE_OUTER_BOUND('',#844,.T.) ;
#569 = FACE_OUTER_BOUND('',#845,.T.) ;
#570 = FACE_OUTER_BOUND('',#846,.T.) ;
#571 = EDGE_LOOP('',(#2555,#2556,#2557,#2558)) ;
#572 = EDGE_LOOP('',(#2559,#2560,#2561,#2562)) ;
#573 = EDGE_LOOP('',(#2563,#2564,#2565,#2566)) ;
#574 = EDGE_LOOP('',(#2567,#2568,#2569,#2570)) ;
#575 = EDGE_LOOP('',(#2571,#2572,#2573,#2574)) ;
#576 = EDGE_LOOP('',(#2575,#2576,#2577,#2578)) ;
#577 = EDGE_LOOP('',(#2579,#2580,#2581,#2582)) ;
#578 = EDGE_LOOP('',(#2583,#2584,#2585,#2586)) ;
#579 = EDGE_LOOP('',(#2587,#2588,#2589,#2590)) ;
#580 = EDGE_LOOP('',(#2591,#2592,#2593,#2594)) ;
#581 = EDGE_LOOP('',(#2595,#2596,#2597,#2598)) ;
#582 = EDGE_LOOP('',(#2599,#2600,#2601,#2602,#2603,#2604,#2605,#2606,#2607,
#2608,#2609,#2610,#2611,#2612,#2613,#2614,#2615,#2616,#2617,#2618,#2619,
#2620,#2621,#2622,#2623,#2624)) ;
#583 = EDGE_LOOP('',(#2625,#2626,#2627,#2628)) ;
#584 = EDGE_LOOP('',(#2629,#2630,#2631,#2632)) ;
#585 = EDGE_LOOP('',(#2633,#2634,#2635)) ;
#586 = EDGE_LOOP('',(#2636,#2637,#2638,#2639)) ;
#587 = EDGE_LOOP('',(#2640,#2641,#2642)) ;
#588 = EDGE_LOOP('',(#2643,#2644,#2645,#2646)) ;
#589 = EDGE_LOOP('',(#2647,#2648,#2649)) ;
#590 = EDGE_LOOP('',(#2650,#2651,#2652,#2653)) ;
#591 = EDGE_LOOP('',(#2654,#2655,#2656)) ;
#592 = EDGE_LOOP('',(#2657,#2658,#2659,#2660)) ;
#593 = EDGE_LOOP('',(#2661,#2662,#2663,#2664)) ;
#594 = EDGE_LOOP('',(#2665,#2666,#2667,#2668)) ;
#595 = EDGE_LOOP('',(#2669,#2670,#2671,#2672)) ;
#596 = EDGE_LOOP('',(#2673,#2674,#2675,#2676)) ;
#597 = EDGE_LOOP('',(#2677,#2678,#2679)) ;
#598 = EDGE_LOOP('',(#2680,#2681,#2682,#2683)) ;
#599 = EDGE_LOOP('',(#2684,#2685,#2686)) ;
#600 = EDGE_LOOP('',(#2687,#2688,#2689,#2690)) ;
#601 = EDGE_LOOP('',(#2691,#2692,#2693,#2694)) ;
#602 = EDGE_LOOP('',(#2695,#2696,#2697,#2698)) ;
#603 = EDGE_LOOP('',(#2699,#2700,#2701,#2702)) ;
#604 = EDGE_LOOP('',(#2703,#2704,#2705,#2706)) ;
#605 = EDGE_LOOP('',(#2707,#2708,#2709)) ;
#606 = EDGE_LOOP('',(#2710,#2711,#2712,#2713)) ;
#607 = EDGE_LOOP('',(#2714,#2715,#2716)) ;
#608 = EDGE_LOOP('',(#2717,#2718,#2719,#2720)) ;
#609 = EDGE_LOOP('',(#2721,#2722,#2723)) ;
#610 = EDGE_LOOP('',(#2724,#2725,#2726,#2727)) ;
#611 = EDGE_LOOP('',(#2728,#2729,#2730)) ;
#612 = EDGE_LOOP('',(#2731,#2732,#2733,#2734)) ;
#613 = EDGE_LOOP('',(#2735,#2736,#2737,#2738)) ;
#614 = EDGE_LOOP('',(#2739,#2740,#2741,#2742)) ;
#615 = EDGE_LOOP('',(#2743,#2744,#2745,#2746)) ;
#616 = EDGE_LOOP('',(#2747,#2748,#2749,#2750,#2751,#2752,#2753,#2754,#2755,
#2756,#2757,#2758,#2759,#2760,#2761,#2762,#2763,#2764,#2765,#2766,#2767,
#2768,#2769,#2770,#2771,#2772)) ;
#617 = EDGE_LOOP('',(#2773,#2774,#2775,#2776)) ;
#618 = EDGE_LOOP('',(#2777,#2778,#2779,#2780)) ;
#619 = EDGE_LOOP('',(#2781,#2782,#2783,#2784)) ;
#620 = EDGE_LOOP('',(#2785,#2786,#2787,#2788)) ;
#621 = EDGE_LOOP('',(#2789,#2790,#2791,#2792)) ;
#622 = EDGE_LOOP('',(#2793,#2794,#2795,#2796)) ;
#623 = EDGE_LOOP('',(#2797,#2798,#2799,#2800)) ;
#624 = EDGE_LOOP('',(#2801,#2802,#2803,#2804)) ;
#625 = EDGE_LOOP('',(#2805,#2806,#2807,#2808)) ;
#626 = EDGE_LOOP('',(#2809,#2810,#2811,#2812)) ;
#627 = EDGE_LOOP('',(#2813,#2814,#2815,#2816,#2817,#2818,#2819,#2820)) ;
#628 = EDGE_LOOP('',(#2821)) ;
#629 = EDGE_LOOP('',(#2822)) ;
#630 = EDGE_LOOP('',(#2823,#2824,#2825,#2826,#2827,#2828,#2829,#2830)) ;
#631 = EDGE_LOOP('',(#2831)) ;
#632 = EDGE_LOOP('',(#2832)) ;
#633 = EDGE_LOOP('',(#2833,#2834,#2835,#2836)) ;
#634 = EDGE_LOOP('',(#2837,#2838,#2839,#2840)) ;
#635 = EDGE_LOOP('',(#2841,#2842,#2843,#2844)) ;
#636 = EDGE_LOOP('',(#2845,#2846,#2847,#2848)) ;
#637 = EDGE_LOOP('',(#2849,#2850,#2851,#2852)) ;
#638 = EDGE_LOOP('',(#2853)) ;
#639 = EDGE_LOOP('',(#2854)) ;
#640 = EDGE_LOOP('',(#2855,#2856,#2857,#2858)) ;
#641 = EDGE_LOOP('',(#2859,#2860,#2861,#2862)) ;
#642 = EDGE_LOOP('',(#2863,#2864,#2865,#2866)) ;
#643 = EDGE_LOOP('',(#2867,#2868,#2869,#2870)) ;
#644 = EDGE_LOOP('',(#2871,#2872,#2873,#2874)) ;
#645 = EDGE_LOOP('',(#2875,#2876,#2877,#2878)) ;
#646 = EDGE_LOOP('',(#2879,#2880,#2881,#2882)) ;
#647 = EDGE_LOOP('',(#2883,#2884,#2885,#2886)) ;
#648 = EDGE_LOOP('',(#2887,#2888,#2889,#2890)) ;
#649 = EDGE_LOOP('',(#2891)) ;
#650 = EDGE_LOOP('',(#2892)) ;
#651 = EDGE_LOOP('',(#2893,#2894,#2895,#2896)) ;
#652 = EDGE_LOOP('',(#2897,#2898,#2899,#2900)) ;
#653 = EDGE_LOOP('',(#2901,#2902,#2903,#2904)) ;
#654 = EDGE_LOOP('',(#2905,#2906,#2907,#2908)) ;
#655 = EDGE_LOOP('',(#2909,#2910,#2911,#2912)) ;
#656 = EDGE_LOOP('',(#2913,#2914,#2915,#2916)) ;
#657 = EDGE_LOOP('',(#2917,#2918,#2919,#2920)) ;
#658 = EDGE_LOOP('',(#2921,#2922,#2923,#2924)) ;
#659 = EDGE_LOOP('',(#2925,#2926,#2927,#2928)) ;
#660 = EDGE_LOOP('',(#2929,#2930,#2931,#2932)) ;
#661 = EDGE_LOOP('',(#2933,#2934,#2935,#2936)) ;
#662 = EDGE_LOOP('',(#2937,#2938,#2939)) ;
#663 = EDGE_LOOP('',(#2940,#2941,#2942,#2943)) ;
#664 = EDGE_LOOP('',(#2944,#2945,#2946)) ;
#665 = EDGE_LOOP('',(#2947,#2948,#2949,#2950)) ;
#666 = EDGE_LOOP('',(#2951,#2952,#2953)) ;
#667 = EDGE_LOOP('',(#2954,#2955,#2956,#2957)) ;
#668 = EDGE_LOOP('',(#2958,#2959,#2960)) ;
#669 = EDGE_LOOP('',(#2961,#2962,#2963,#2964)) ;
#670 = EDGE_LOOP('',(#2965,#2966,#2967,#2968)) ;
#671 = EDGE_LOOP('',(#2969,#2970,#2971,#2972)) ;
#672 = EDGE_LOOP('',(#2973,#2974,#2975,#2976)) ;
#673 = EDGE_LOOP('',(#2977,#2978,#2979,#2980)) ;
#674 = EDGE_LOOP('',(#2981,#2982,#2983)) ;
#675 = EDGE_LOOP('',(#2984,#2985,#2986,#2987)) ;
#676 = EDGE_LOOP('',(#2988,#2989,#2990)) ;
#677 = EDGE_LOOP('',(#2991,#2992,#2993,#2994)) ;
#678 = EDGE_LOOP('',(#2995,#2996,#2997,#2998)) ;
#679 = EDGE_LOOP('',(#2999,#3000,#3001,#3002)) ;
#680 = EDGE_LOOP('',(#3003,#3004,#3005,#3006)) ;
#681 = EDGE_LOOP('',(#3007,#3008,#3009,#3010)) ;
#682 = EDGE_LOOP('',(#3011,#3012,#3013)) ;
#683 = EDGE_LOOP('',(#3014,#3015,#3016,#3017)) ;
#684 = EDGE_LOOP('',(#3018,#3019,#3020)) ;
#685 = EDGE_LOOP('',(#3021,#3022,#3023,#3024)) ;
#686 = EDGE_LOOP('',(#3025,#3026,#3027)) ;
#687 = EDGE_LOOP('',(#3028,#3029,#3030,#3031)) ;
#688 = EDGE_LOOP('',(#3032,#3033,#3034)) ;
#689 = EDGE_LOOP('',(#3035,#3036,#3037,#3038)) ;
#690 = EDGE_LOOP('',(#3039,#3040,#3041,#3042)) ;
#691 = EDGE_LOOP('',(#3043,#3044,#3045,#3046)) ;
#692 = EDGE_LOOP('',(#3047,#3048,#3049,#3050)) ;
#693 = EDGE_LOOP('',(#3051,#3052,#3053,#3054)) ;
#694 = EDGE_LOOP('',(#3055,#3056,#3057,#3058)) ;
#695 = EDGE_LOOP('',(#3059,#3060,#3061,#3062)) ;
#696 = EDGE_LOOP('',(#3063,#3064,#3065,#3066,#3067,#3068,#3069,#3070,#3071,
#3072,#3073,#3074,#3075,#3076,#3077,#3078)) ;
#697 = EDGE_LOOP('',(#3079,#3080,#3081,#3082)) ;
#698 = EDGE_LOOP('',(#3083,#3084,#3085,#3086)) ;
#699 = EDGE_LOOP('',(#3087,#3088,#3089,#3090)) ;
#700 = EDGE_LOOP('',(#3091,#3092,#3093,#3094)) ;
#701 = EDGE_LOOP('',(#3095,#3096,#3097,#3098)) ;
#702 = EDGE_LOOP('',(#3099,#3100,#3101,#3102)) ;
#703 = EDGE_LOOP('',(#3103,#3104,#3105,#3106)) ;
#704 = EDGE_LOOP('',(#3107,#3108,#3109,#3110)) ;
#705 = EDGE_LOOP('',(#3111,#3112,#3113,#3114)) ;
#706 = EDGE_LOOP('',(#3115,#3116,#3117,#3118)) ;
#707 = EDGE_LOOP('',(#3119,#3120,#3121,#3122)) ;
#708 = EDGE_LOOP('',(#3123,#3124,#3125,#3126)) ;
#709 = EDGE_LOOP('',(#3127,#3128,#3129,#3130)) ;
#710 = EDGE_LOOP('',(#3131,#3132,#3133,#3134,#3135,#3136,#3137,#3138,#3139,
#3140,#3141,#3142,#3143,#3144,#3145,#3146)) ;
#711 = EDGE_LOOP('',(#3147,#3148,#3149,#3150)) ;
#712 = EDGE_LOOP('',(#3151,#3152,#3153,#3154)) ;
#713 = EDGE_LOOP('',(#3155,#3156,#3157,#3158)) ;
#714 = EDGE_LOOP('',(#3159,#3160,#3161,#3162)) ;
#715 = EDGE_LOOP('',(#3163,#3164,#3165,#3166)) ;
#716 = EDGE_LOOP('',(#3167,#3168,#3169,#3170)) ;
#717 = EDGE_LOOP('',(#3171,#3172,#3173,#3174)) ;
#718 = EDGE_LOOP('',(#3175,#3176,#3177,#3178,#3179,#3180,#3181,#3182)) ;
#719 = EDGE_LOOP('',(#3183)) ;
#720 = EDGE_LOOP('',(#3184)) ;
#721 = EDGE_LOOP('',(#3185,#3186,#3187,#3188,#3189,#3190,#3191,#3192)) ;
#722 = EDGE_LOOP('',(#3193)) ;
#723 = EDGE_LOOP('',(#3194)) ;
#724 = EDGE_LOOP('',(#3195,#3196,#3197,#3198)) ;
#725 = EDGE_LOOP('',(#3199,#3200,#3201,#3202)) ;
#726 = EDGE_LOOP('',(#3203,#3204,#3205,#3206)) ;
#727 = EDGE_LOOP('',(#3207,#3208,#3209,#3210)) ;
#728 = EDGE_LOOP('',(#3211,#3212,#3213,#3214)) ;
#729 = EDGE_LOOP('',(#3215,#3216,#3217,#3218)) ;
#730 = EDGE_LOOP('',(#3219,#3220,#3221,#3222)) ;
#731 = EDGE_LOOP('',(#3223,#3224,#3225,#3226)) ;
#732 = EDGE_LOOP('',(#3227,#3228,#3229,#3230)) ;
#733 = EDGE_LOOP('',(#3231,#3232,#3233,#3234)) ;
#734 = EDGE_LOOP('',(#3235,#3236,#3237,#3238)) ;
#735 = EDGE_LOOP('',(#3239,#3240,#3241,#3242)) ;
#736 = EDGE_LOOP('',(#3243,#3244,#3245,#3246)) ;
#737 = EDGE_LOOP('',(#3247,#3248,#3249,#3250)) ;
#738 = EDGE_LOOP('',(#3251,#3252,#3253,#3254)) ;
#739 = EDGE_LOOP('',(#3255,#3256,#3257,#3258)) ;
#740 = EDGE_LOOP('',(#3259,#3260,#3261,#3262)) ;
#741 = EDGE_LOOP('',(#3263,#3264,#3265,#3266,#3267)) ;
#742 = EDGE_LOOP('',(#3268,#3269,#3270,#3271,#3272)) ;
#743 = EDGE_LOOP('',(#3273,#3274,#3275,#3276,#3277)) ;
#744 = EDGE_LOOP('',(#3278,#3279,#3280,#3281)) ;
#745 = EDGE_LOOP('',(#3282)) ;
#746 = EDGE_LOOP('',(#3283)) ;
#747 = EDGE_LOOP('',(#3284,#3285,#3286,#3287,#3288)) ;
#748 = EDGE_LOOP('',(#3289,#3290,#3291,#3292,#3293)) ;
#749 = EDGE_LOOP('',(#3294,#3295,#3296,#3297,#3298)) ;
#750 = EDGE_LOOP('',(#3299,#3300,#3301,#3302,#3303)) ;
#751 = EDGE_LOOP('',(#3304,#3305,#3306,#3307)) ;
#752 = EDGE_LOOP('',(#3308)) ;
#753 = EDGE_LOOP('',(#3309)) ;
#754 = EDGE_LOOP('',(#3310,#3311,#3312,#3313,#3314)) ;
#755 = EDGE_LOOP('',(#3315,#3316,#3317,#3318)) ;
#756 = EDGE_LOOP('',(#3319,#3320,#3321,#3322)) ;
#757 = EDGE_LOOP('',(#3323)) ;
#758 = EDGE_LOOP('',(#3324)) ;
#759 = EDGE_LOOP('',(#3325)) ;
#760 = EDGE_LOOP('',(#3326)) ;
#761 = EDGE_LOOP('',(#3327,#3328,#3329,#3330)) ;
#762 = EDGE_LOOP('',(#3331,#3332,#3333,#3334)) ;
#763 = EDGE_LOOP('',(#3335)) ;
#764 = EDGE_LOOP('',(#3336)) ;
#765 = EDGE_LOOP('',(#3337)) ;
#766 = EDGE_LOOP('',(#3338)) ;
#767 = EDGE_LOOP('',(#3339,#3340,#3341,#3342)) ;
#768 = EDGE_LOOP('',(#3343,#3344,#3345,#3346)) ;
#769 = EDGE_LOOP('',(#3347)) ;
#770 = EDGE_LOOP('',(#3348)) ;
#771 = EDGE_LOOP('',(#3349)) ;
#772 = EDGE_LOOP('',(#3350)) ;
#773 = EDGE_LOOP('',(#3351,#3352,#3353,#3354)) ;
#774 = EDGE_LOOP('',(#3355,#3356,#3357,#3358)) ;
#775 = EDGE_LOOP('',(#3359)) ;
#776 = EDGE_LOOP('',(#3360)) ;
#777 = EDGE_LOOP('',(#3361)) ;
#778 = EDGE_LOOP('',(#3362)) ;
#779 = EDGE_LOOP('',(#3363,#3364,#3365,#3366)) ;
#780 = EDGE_LOOP('',(#3367,#3368,#3369,#3370)) ;
#781 = EDGE_LOOP('',(#3371,#3372,#3373,#3374)) ;
#782 = EDGE_LOOP('',(#3375,#3376,#3377,#3378,#3379,#3380)) ;
#783 = EDGE_LOOP('',(#3381,#3382,#3383,#3384)) ;
#784 = EDGE_LOOP('',(#3385,#3386,#3387,#3388)) ;
#785 = EDGE_LOOP('',(#3389,#3390,#3391,#3392)) ;
#786 = EDGE_LOOP('',(#3393)) ;
#787 = EDGE_LOOP('',(#3394,#3395,#3396,#3397,#3398,#3399)) ;
#788 = EDGE_LOOP('',(#3400)) ;
#789 = EDGE_LOOP('',(#3401)) ;
#790 = EDGE_LOOP('',(#3402)) ;
#791 = EDGE_LOOP('',(#3403,#3404,#3405,#3406)) ;
#792 = EDGE_LOOP('',(#3407,#3408,#3409,#3410)) ;
#793 = EDGE_LOOP('',(#3411,#3412,#3413,#3414)) ;
#794 = EDGE_LOOP('',(#3415,#3416,#3417,#3418)) ;
#795 = EDGE_LOOP('',(#3419,#3420,#3421,#3422)) ;
#796 = EDGE_LOOP('',(#3423,#3424,#3425,#3426)) ;
#797 = EDGE_LOOP('',(#3427,#3428,#3429,#3430)) ;
#798 = EDGE_LOOP('',(#3431,#3432,#3433,#3434)) ;
#799 = EDGE_LOOP('',(#3435,#3436,#3437,#3438,#3439,#3440)) ;
#800 = EDGE_LOOP('',(#3441,#3442,#3443,#3444)) ;
#801 = EDGE_LOOP('',(#3445,#3446,#3447,#3448)) ;
#802 = EDGE_LOOP('',(#3449,#3450,#3451,#3452)) ;
#803 = EDGE_LOOP('',(#3453)) ;
#804 = EDGE_LOOP('',(#3454,#3455,#3456,#3457,#3458,#3459)) ;
#805 = EDGE_LOOP('',(#3460)) ;
#806 = EDGE_LOOP('',(#3461)) ;
#807 = EDGE_LOOP('',(#3462)) ;
#808 = EDGE_LOOP('',(#3463,#3464,#3465,#3466)) ;
#809 = EDGE_LOOP('',(#3467,#3468,#3469,#3470)) ;
#810 = EDGE_LOOP('',(#3471,#3472,#3473,#3474)) ;
#811 = EDGE_LOOP('',(#3475,#3476,#3477,#3478)) ;
#812 = EDGE_LOOP('',(#3479,#3480,#3481,#3482)) ;
#813 = EDGE_LOOP('',(#3483,#3484,#3485,#3486)) ;
#814 = EDGE_LOOP('',(#3487,#3488,#3489,#3490)) ;
#815 = EDGE_LOOP('',(#3491,#3492,#3493,#3494)) ;
#816 = EDGE_LOOP('',(#3495,#3496,#3497,#3498,#3499,#3500)) ;
#817 = EDGE_LOOP('',(#3501,#3502,#3503,#3504)) ;
#818 = EDGE_LOOP('',(#3505,#3506,#3507,#3508)) ;
#819 = EDGE_LOOP('',(#3509,#3510,#3511,#3512)) ;
#820 = EDGE_LOOP('',(#3513)) ;
#821 = EDGE_LOOP('',(#3514,#3515,#3516,#3517,#3518,#3519)) ;
#822 = EDGE_LOOP('',(#3520)) ;
#823 = EDGE_LOOP('',(#3521)) ;
#824 = EDGE_LOOP('',(#3522)) ;
#825 = EDGE_LOOP('',(#3523,#3524,#3525,#3526)) ;
#826 = EDGE_LOOP('',(#3527,#3528,#3529,#3530)) ;
#827 = EDGE_LOOP('',(#3531,#3532,#3533,#3534)) ;
#828 = EDGE_LOOP('',(#3535,#3536,#3537,#3538)) ;
#829 = EDGE_LOOP('',(#3539,#3540,#3541,#3542)) ;
#830 = EDGE_LOOP('',(#3543,#3544,#3545,#3546)) ;
#831 = EDGE_LOOP('',(#3547,#3548,#3549,#3550)) ;
#832 = EDGE_LOOP('',(#3551,#3552,#3553,#3554)) ;
#833 = EDGE_LOOP('',(#3555,#3556,#3557,#3558,#3559,#3560)) ;
#834 = EDGE_LOOP('',(#3561,#3562,#3563,#3564)) ;
#835 = EDGE_LOOP('',(#3565,#3566,#3567,#3568)) ;
#836 = EDGE_LOOP('',(#3569,#3570,#3571,#3572)) ;
#837 = EDGE_LOOP('',(#3573)) ;
#838 = EDGE_LOOP('',(#3574,#3575,#3576,#3577,#3578,#3579)) ;
#839 = EDGE_LOOP('',(#3580)) ;
#840 = EDGE_LOOP('',(#3581)) ;
#841 = EDGE_LOOP('',(#3582)) ;
#842 = EDGE_LOOP('',(#3583,#3584,#3585,#3586)) ;
#843 = EDGE_LOOP('',(#3587,#3588,#3589,#3590)) ;
#844 = EDGE_LOOP('',(#3591,#3592,#3593,#3594)) ;
#845 = EDGE_LOOP('',(#3595,#3596,#3597,#3598)) ;
#846 = EDGE_LOOP('',(#3599,#3600,#3601,#3602)) ;
#847 = LINE('',#5646,#1207) ;
#848 = LINE('',#5649,#1208) ;
#849 = LINE('',#5674,#1209) ;
#850 = LINE('',#5678,#1210) ;
#851 = LINE('',#5684,#1211) ;
#852 = LINE('',#5688,#1212) ;
#853 = LINE('',#5694,#1213) ;
#854 = LINE('',#5698,#1214) ;
#855 = LINE('',#5704,#1215) ;
#856 = LINE('',#5708,#1216) ;
#857 = LINE('',#5712,#1217) ;
#858 = LINE('',#5714,#1218) ;
#859 = LINE('',#5716,#1219) ;
#860 = LINE('',#5720,#1220) ;
#861 = LINE('',#5722,#1221) ;
#862 = LINE('',#5724,#1222) ;
#863 = LINE('',#5726,#1223) ;
#864 = LINE('',#5728,#1224) ;
#865 = LINE('',#5732,#1225) ;
#866 = LINE('',#5736,#1226) ;
#867 = LINE('',#5738,#1227) ;
#868 = LINE('',#5740,#1228) ;
#869 = LINE('',#5744,#1229) ;
#870 = LINE('',#5748,#1230) ;
#871 = LINE('',#5750,#1231) ;
#872 = LINE('',#5752,#1232) ;
#873 = LINE('',#5754,#1233) ;
#874 = LINE('',#5756,#1234) ;
#875 = LINE('',#5759,#1235) ;
#876 = LINE('',#5762,#1236) ;
#877 = LINE('',#5765,#1237) ;
#878 = LINE('',#5768,#1238) ;
#879 = LINE('',#5769,#1239) ;
#880 = LINE('',#5773,#1240) ;
#881 = LINE('',#5776,#1241) ;
#882 = LINE('',#5777,#1242) ;
#883 = LINE('',#5781,#1243) ;
#884 = LINE('',#5784,#1244) ;
#885 = LINE('',#5785,#1245) ;
#886 = LINE('',#5789,#1246) ;
#887 = LINE('',#5792,#1247) ;
#888 = LINE('',#5793,#1248) ;
#889 = LINE('',#5797,#1249) ;
#890 = LINE('',#5800,#1250) ;
#891 = LINE('',#5801,#1251) ;
#892 = LINE('',#5805,#1252) ;
#893 = LINE('',#5808,#1253) ;
#894 = LINE('',#5809,#1254) ;
#895 = LINE('',#5813,#1255) ;
#896 = LINE('',#5816,#1256) ;
#897 = LINE('',#5817,#1257) ;
#898 = LINE('',#5821,#1258) ;
#899 = LINE('',#5824,#1259) ;
#900 = LINE('',#5825,#1260) ;
#901 = LINE('',#5829,#1261) ;
#902 = LINE('',#5832,#1262) ;
#903 = LINE('',#5833,#1263) ;
#904 = LINE('',#5837,#1264) ;
#905 = LINE('',#5840,#1265) ;
#906 = LINE('',#5841,#1266) ;
#907 = LINE('',#5845,#1267) ;
#908 = LINE('',#5848,#1268) ;
#909 = LINE('',#5849,#1269) ;
#910 = LINE('',#5853,#1270) ;
#911 = LINE('',#5856,#1271) ;
#912 = LINE('',#5857,#1272) ;
#913 = LINE('',#5861,#1273) ;
#914 = LINE('',#5864,#1274) ;
#915 = LINE('',#5865,#1275) ;
#916 = LINE('',#5869,#1276) ;
#917 = LINE('',#5872,#1277) ;
#918 = LINE('',#5873,#1278) ;
#919 = LINE('',#5877,#1279) ;
#920 = LINE('',#5880,#1280) ;
#921 = LINE('',#5881,#1281) ;
#922 = LINE('',#5885,#1282) ;
#923 = LINE('',#5888,#1283) ;
#924 = LINE('',#5889,#1284) ;
#925 = LINE('',#5892,#1285) ;
#926 = LINE('',#5893,#1286) ;
#927 = LINE('',#5897,#1287) ;
#928 = LINE('',#5901,#1288) ;
#929 = LINE('',#5903,#1289) ;
#930 = LINE('',#5905,#1290) ;
#931 = LINE('',#5907,#1291) ;
#932 = LINE('',#5909,#1292) ;
#933 = LINE('',#5913,#1293) ;
#934 = LINE('',#5917,#1294) ;
#935 = LINE('',#5919,#1295) ;
#936 = LINE('',#5921,#1296) ;
#937 = LINE('',#5925,#1297) ;
#938 = LINE('',#5929,#1298) ;
#939 = LINE('',#5931,#1299) ;
#940 = LINE('',#5933,#1300) ;
#941 = LINE('',#5935,#1301) ;
#942 = LINE('',#5937,#1302) ;
#943 = LINE('',#5941,#1303) ;
#944 = LINE('',#5942,#1304) ;
#945 = LINE('',#5943,#1305) ;
#946 = LINE('',#5948,#1306) ;
#947 = LINE('',#5949,#1307) ;
#948 = LINE('',#5954,#1308) ;
#949 = LINE('',#5955,#1309) ;
#950 = LINE('',#5960,#1310) ;
#951 = LINE('',#5961,#1311) ;
#952 = LINE('',#5966,#1312) ;
#953 = LINE('',#5967,#1313) ;
#954 = LINE('',#5972,#1314) ;
#955 = LINE('',#5973,#1315) ;
#956 = LINE('',#5978,#1316) ;
#957 = LINE('',#5979,#1317) ;
#958 = LINE('',#5982,#1318) ;
#959 = LINE('',#5983,#1319) ;
#960 = LINE('',#5985,#1320) ;
#961 = LINE('',#5987,#1321) ;
#962 = LINE('',#5990,#1322) ;
#963 = LINE('',#5991,#1323) ;
#964 = LINE('',#5993,#1324) ;
#965 = LINE('',#5995,#1325) ;
#966 = LINE('',#5998,#1326) ;
#967 = LINE('',#6000,#1327) ;
#968 = LINE('',#6004,#1328) ;
#969 = LINE('',#6005,#1329) ;
#970 = LINE('',#6008,#1330) ;
#971 = LINE('',#6012,#1331) ;
#972 = LINE('',#6013,#1332) ;
#973 = LINE('',#6016,#1333) ;
#974 = LINE('',#6017,#1334) ;
#975 = LINE('',#6022,#1335) ;
#976 = LINE('',#6023,#1336) ;
#977 = LINE('',#6026,#1337) ;
#978 = LINE('',#6030,#1338) ;
#979 = LINE('',#6031,#1339) ;
#980 = LINE('',#6034,#1340) ;
#981 = LINE('',#6035,#1341) ;
#982 = LINE('',#6040,#1342) ;
#983 = LINE('',#6041,#1343) ;
#984 = LINE('',#6044,#1344) ;
#985 = LINE('',#6048,#1345) ;
#986 = LINE('',#6049,#1346) ;
#987 = LINE('',#6052,#1347) ;
#988 = LINE('',#6056,#1348) ;
#989 = LINE('',#6057,#1349) ;
#990 = LINE('',#6060,#1350) ;
#991 = LINE('',#6064,#1351) ;
#992 = LINE('',#6065,#1352) ;
#993 = LINE('',#6068,#1353) ;
#994 = LINE('',#6069,#1354) ;
#995 = LINE('',#6074,#1355) ;
#996 = LINE('',#6075,#1356) ;
#997 = LINE('',#6078,#1357) ;
#998 = LINE('',#6079,#1358) ;
#999 = LINE('',#6083,#1359) ;
#1000 = LINE('',#6084,#1360) ;
#1001 = LINE('',#6086,#1361) ;
#1002 = LINE('',#6088,#1362) ;
#1003 = LINE('',#6090,#1363) ;
#1004 = LINE('',#6092,#1364) ;
#1005 = LINE('',#6094,#1365) ;
#1006 = LINE('',#6096,#1366) ;
#1007 = LINE('',#6098,#1367) ;
#1008 = LINE('',#6100,#1368) ;
#1009 = LINE('',#6102,#1369) ;
#1010 = LINE('',#6104,#1370) ;
#1011 = LINE('',#6106,#1371) ;
#1012 = LINE('',#6108,#1372) ;
#1013 = LINE('',#6110,#1373) ;
#1014 = LINE('',#6112,#1374) ;
#1015 = LINE('',#6114,#1375) ;
#1016 = LINE('',#6116,#1376) ;
#1017 = LINE('',#6118,#1377) ;
#1018 = LINE('',#6120,#1378) ;
#1019 = LINE('',#6122,#1379) ;
#1020 = LINE('',#6124,#1380) ;
#1021 = LINE('',#6126,#1381) ;
#1022 = LINE('',#6128,#1382) ;
#1023 = LINE('',#6130,#1383) ;
#1024 = LINE('',#6132,#1384) ;
#1025 = LINE('',#6134,#1385) ;
#1026 = LINE('',#6136,#1386) ;
#1027 = LINE('',#6138,#1387) ;
#1028 = LINE('',#6140,#1388) ;
#1029 = LINE('',#6142,#1389) ;
#1030 = LINE('',#6144,#1390) ;
#1031 = LINE('',#6165,#1391) ;
#1032 = LINE('',#6168,#1392) ;
#1033 = LINE('',#6183,#1393) ;
#1034 = LINE('',#6185,#1394) ;
#1035 = LINE('',#6187,#1395) ;
#1036 = LINE('',#6191,#1396) ;
#1037 = LINE('',#6195,#1397) ;
#1038 = LINE('',#6199,#1398) ;
#1039 = LINE('',#6203,#1399) ;
#1040 = LINE('',#6207,#1400) ;
#1041 = LINE('',#6210,#1401) ;
#1042 = LINE('',#6213,#1402) ;
#1043 = LINE('',#6216,#1403) ;
#1044 = LINE('',#6219,#1404) ;
#1045 = LINE('',#6220,#1405) ;
#1046 = LINE('',#6224,#1406) ;
#1047 = LINE('',#6227,#1407) ;
#1048 = LINE('',#6228,#1408) ;
#1049 = LINE('',#6232,#1409) ;
#1050 = LINE('',#6235,#1410) ;
#1051 = LINE('',#6236,#1411) ;
#1052 = LINE('',#6240,#1412) ;
#1053 = LINE('',#6243,#1413) ;
#1054 = LINE('',#6244,#1414) ;
#1055 = LINE('',#6248,#1415) ;
#1056 = LINE('',#6251,#1416) ;
#1057 = LINE('',#6252,#1417) ;
#1058 = LINE('',#6256,#1418) ;
#1059 = LINE('',#6259,#1419) ;
#1060 = LINE('',#6260,#1420) ;
#1061 = LINE('',#6263,#1421) ;
#1062 = LINE('',#6264,#1422) ;
#1063 = LINE('',#6268,#1423) ;
#1064 = LINE('',#6272,#1424) ;
#1065 = LINE('',#6276,#1425) ;
#1066 = LINE('',#6280,#1426) ;
#1067 = LINE('',#6284,#1427) ;
#1068 = LINE('',#6288,#1428) ;
#1069 = LINE('',#6292,#1429) ;
#1070 = LINE('',#6293,#1430) ;
#1071 = LINE('',#6294,#1431) ;
#1072 = LINE('',#6299,#1432) ;
#1073 = LINE('',#6300,#1433) ;
#1074 = LINE('',#6303,#1434) ;
#1075 = LINE('',#6305,#1435) ;
#1076 = LINE('',#6309,#1436) ;
#1077 = LINE('',#6310,#1437) ;
#1078 = LINE('',#6313,#1438) ;
#1079 = LINE('',#6314,#1439) ;
#1080 = LINE('',#6317,#1440) ;
#1081 = LINE('',#6320,#1441) ;
#1082 = LINE('',#6324,#1442) ;
#1083 = LINE('',#6327,#1443) ;
#1084 = LINE('',#6328,#1444) ;
#1085 = LINE('',#6335,#1445) ;
#1086 = LINE('',#6336,#1446) ;
#1087 = LINE('',#6343,#1447) ;
#1088 = LINE('',#6344,#1448) ;
#1089 = LINE('',#6347,#1449) ;
#1090 = LINE('',#6351,#1450) ;
#1091 = LINE('',#6352,#1451) ;
#1092 = LINE('',#6355,#1452) ;
#1093 = LINE('',#6358,#1453) ;
#1094 = LINE('',#6359,#1454) ;
#1095 = LINE('',#6361,#1455) ;
#1096 = LINE('',#6362,#1456) ;
#1097 = LINE('',#6364,#1457) ;
#1098 = LINE('',#6366,#1458) ;
#1099 = LINE('',#6368,#1459) ;
#1100 = LINE('',#6370,#1460) ;
#1101 = LINE('',#6372,#1461) ;
#1102 = LINE('',#6374,#1462) ;
#1103 = LINE('',#6376,#1463) ;
#1104 = LINE('',#6378,#1464) ;
#1105 = LINE('',#6379,#1465) ;
#1106 = LINE('',#6381,#1466) ;
#1107 = LINE('',#6388,#1467) ;
#1108 = LINE('',#6392,#1468) ;
#1109 = LINE('',#6398,#1469) ;
#1110 = LINE('',#6404,#1470) ;
#1111 = LINE('',#6409,#1471) ;
#1112 = LINE('',#6413,#1472) ;
#1113 = LINE('',#6419,#1473) ;
#1114 = LINE('',#6425,#1474) ;
#1115 = LINE('',#6431,#1475) ;
#1116 = LINE('',#6437,#1476) ;
#1117 = LINE('',#6446,#1477) ;
#1118 = LINE('',#6452,#1478) ;
#1119 = LINE('',#6461,#1479) ;
#1120 = LINE('',#6467,#1480) ;
#1121 = LINE('',#6476,#1481) ;
#1122 = LINE('',#6482,#1482) ;
#1123 = LINE('',#6490,#1483) ;
#1124 = LINE('',#6492,#1484) ;
#1125 = LINE('',#6494,#1485) ;
#1126 = LINE('',#6495,#1486) ;
#1127 = LINE('',#6499,#1487) ;
#1128 = LINE('',#6500,#1488) ;
#1129 = LINE('',#6501,#1489) ;
#1130 = LINE('',#6504,#1490) ;
#1131 = LINE('',#6506,#1491) ;
#1132 = LINE('',#6507,#1492) ;
#1133 = LINE('',#6510,#1493) ;
#1134 = LINE('',#6512,#1494) ;
#1135 = LINE('',#6513,#1495) ;
#1136 = LINE('',#6516,#1496) ;
#1137 = LINE('',#6517,#1497) ;
#1138 = LINE('',#6520,#1498) ;
#1139 = LINE('',#6521,#1499) ;
#1140 = LINE('',#6523,#1500) ;
#1141 = LINE('',#6540,#1501) ;
#1142 = LINE('',#6547,#1502) ;
#1143 = LINE('',#6550,#1503) ;
#1144 = LINE('',#6555,#1504) ;
#1145 = LINE('',#6557,#1505) ;
#1146 = LINE('',#6559,#1506) ;
#1147 = LINE('',#6560,#1507) ;
#1148 = LINE('',#6564,#1508) ;
#1149 = LINE('',#6565,#1509) ;
#1150 = LINE('',#6566,#1510) ;
#1151 = LINE('',#6569,#1511) ;
#1152 = LINE('',#6571,#1512) ;
#1153 = LINE('',#6572,#1513) ;
#1154 = LINE('',#6575,#1514) ;
#1155 = LINE('',#6577,#1515) ;
#1156 = LINE('',#6578,#1516) ;
#1157 = LINE('',#6581,#1517) ;
#1158 = LINE('',#6582,#1518) ;
#1159 = LINE('',#6585,#1519) ;
#1160 = LINE('',#6586,#1520) ;
#1161 = LINE('',#6588,#1521) ;
#1162 = LINE('',#6605,#1522) ;
#1163 = LINE('',#6612,#1523) ;
#1164 = LINE('',#6615,#1524) ;
#1165 = LINE('',#6620,#1525) ;
#1166 = LINE('',#6622,#1526) ;
#1167 = LINE('',#6624,#1527) ;
#1168 = LINE('',#6625,#1528) ;
#1169 = LINE('',#6629,#1529) ;
#1170 = LINE('',#6630,#1530) ;
#1171 = LINE('',#6631,#1531) ;
#1172 = LINE('',#6634,#1532) ;
#1173 = LINE('',#6636,#1533) ;
#1174 = LINE('',#6637,#1534) ;
#1175 = LINE('',#6640,#1535) ;
#1176 = LINE('',#6642,#1536) ;
#1177 = LINE('',#6643,#1537) ;
#1178 = LINE('',#6646,#1538) ;
#1179 = LINE('',#6647,#1539) ;
#1180 = LINE('',#6650,#1540) ;
#1181 = LINE('',#6651,#1541) ;
#1182 = LINE('',#6653,#1542) ;
#1183 = LINE('',#6670,#1543) ;
#1184 = LINE('',#6677,#1544) ;
#1185 = LINE('',#6680,#1545) ;
#1186 = LINE('',#6685,#1546) ;
#1187 = LINE('',#6687,#1547) ;
#1188 = LINE('',#6689,#1548) ;
#1189 = LINE('',#6690,#1549) ;
#1190 = LINE('',#6694,#1550) ;
#1191 = LINE('',#6695,#1551) ;
#1192 = LINE('',#6696,#1552) ;
#1193 = LINE('',#6699,#1553) ;
#1194 = LINE('',#6701,#1554) ;
#1195 = LINE('',#6702,#1555) ;
#1196 = LINE('',#6705,#1556) ;
#1197 = LINE('',#6707,#1557) ;
#1198 = LINE('',#6708,#1558) ;
#1199 = LINE('',#6711,#1559) ;
#1200 = LINE('',#6712,#1560) ;
#1201 = LINE('',#6715,#1561) ;
#1202 = LINE('',#6716,#1562) ;
#1203 = LINE('',#6718,#1563) ;
#1204 = LINE('',#6735,#1564) ;
#1205 = LINE('',#6742,#1565) ;
#1206 = LINE('',#6745,#1566) ;
#1207 = VECTOR('',#4445,1.) ;
#1208 = VECTOR('',#4448,1.) ;
#1209 = VECTOR('',#4461,3.25) ;
#1210 = VECTOR('',#4466,1.) ;
#1211 = VECTOR('',#4473,3.25) ;
#1212 = VECTOR('',#4478,1.) ;
#1213 = VECTOR('',#4485,3.25) ;
#1214 = VECTOR('',#4490,1.) ;
#1215 = VECTOR('',#4497,3.25) ;
#1216 = VECTOR('',#4502,1.) ;
#1217 = VECTOR('',#4507,1.) ;
#1218 = VECTOR('',#4508,1.) ;
#1219 = VECTOR('',#4509,1.) ;
#1220 = VECTOR('',#4512,1.00000000000064) ;
#1221 = VECTOR('',#4513,1.) ;
#1222 = VECTOR('',#4514,1.00000000000064) ;
#1223 = VECTOR('',#4515,1.) ;
#1224 = VECTOR('',#4516,1.00000000000064) ;
#1225 = VECTOR('',#4519,1.) ;
#1226 = VECTOR('',#4522,1.00000000000064) ;
#1227 = VECTOR('',#4523,1.) ;
#1228 = VECTOR('',#4524,1.00000000000064) ;
#1229 = VECTOR('',#4527,1.) ;
#1230 = VECTOR('',#4530,1.00000000000064) ;
#1231 = VECTOR('',#4531,1.) ;
#1232 = VECTOR('',#4532,1.00000000000064) ;
#1233 = VECTOR('',#4533,1.) ;
#1234 = VECTOR('',#4534,1.00000000000064) ;
#1235 = VECTOR('',#4537,1.) ;
#1236 = VECTOR('',#4540,0.999999999999933) ;
#1237 = VECTOR('',#4543,0.99999999999982) ;
#1238 = VECTOR('',#4546,1.00000000000064) ;
#1239 = VECTOR('',#4547,1.00000000000032) ;
#1240 = VECTOR('',#4552,1.00000000000064) ;
#1241 = VECTOR('',#4555,1.) ;
#1242 = VECTOR('',#4556,1.00000000000064) ;
#1243 = VECTOR('',#4561,1.00000000000032) ;
#1244 = VECTOR('',#4564,1.00000000000064) ;
#1245 = VECTOR('',#4565,1.00000000000032) ;
#1246 = VECTOR('',#4570,1.00000000000064) ;
#1247 = VECTOR('',#4573,1.) ;
#1248 = VECTOR('',#4574,1.00000000000064) ;
#1249 = VECTOR('',#4579,1.00000000000032) ;
#1250 = VECTOR('',#4582,1.00000000000064) ;
#1251 = VECTOR('',#4583,1.00000000000032) ;
#1252 = VECTOR('',#4588,0.999999999999933) ;
#1253 = VECTOR('',#4591,1.) ;
#1254 = VECTOR('',#4592,1.00000000000064) ;
#1255 = VECTOR('',#4597,0.99999999999982) ;
#1256 = VECTOR('',#4600,1.00000000000064) ;
#1257 = VECTOR('',#4601,1.00000000000032) ;
#1258 = VECTOR('',#4606,1.00000000000064) ;
#1259 = VECTOR('',#4609,1.) ;
#1260 = VECTOR('',#4610,1.00000000000064) ;
#1261 = VECTOR('',#4615,1.00000000000032) ;
#1262 = VECTOR('',#4618,1.00000000000064) ;
#1263 = VECTOR('',#4619,1.00000000000032) ;
#1264 = VECTOR('',#4624,1.00000000000064) ;
#1265 = VECTOR('',#4627,1.) ;
#1266 = VECTOR('',#4628,1.00000000000064) ;
#1267 = VECTOR('',#4633,1.00000000000032) ;
#1268 = VECTOR('',#4636,1.00000000000064) ;
#1269 = VECTOR('',#4637,1.00000000000032) ;
#1270 = VECTOR('',#4642,1.00000000000064) ;
#1271 = VECTOR('',#4645,1.) ;
#1272 = VECTOR('',#4646,1.00000000000064) ;
#1273 = VECTOR('',#4651,1.00000000000032) ;
#1274 = VECTOR('',#4654,1.00000000000064) ;
#1275 = VECTOR('',#4655,1.00000000000032) ;
#1276 = VECTOR('',#4660,1.00000000000064) ;
#1277 = VECTOR('',#4663,1.) ;
#1278 = VECTOR('',#4664,1.00000000000064) ;
#1279 = VECTOR('',#4669,1.00000000000032) ;
#1280 = VECTOR('',#4672,1.00000000000064) ;
#1281 = VECTOR('',#4673,1.00000000000032) ;
#1282 = VECTOR('',#4678,1.00000000000064) ;
#1283 = VECTOR('',#4681,1.00000000000064) ;
#1284 = VECTOR('',#4682,1.) ;
#1285 = VECTOR('',#4685,1.) ;
#1286 = VECTOR('',#4686,1.00000000000064) ;
#1287 = VECTOR('',#4689,1.) ;
#1288 = VECTOR('',#4692,1.00000000000064) ;
#1289 = VECTOR('',#4693,1.) ;
#1290 = VECTOR('',#4694,1.00000000000064) ;
#1291 = VECTOR('',#4695,1.) ;
#1292 = VECTOR('',#4696,1.00000000000064) ;
#1293 = VECTOR('',#4699,1.) ;
#1294 = VECTOR('',#4702,1.00000000000064) ;
#1295 = VECTOR('',#4703,1.) ;
#1296 = VECTOR('',#4704,1.00000000000064) ;
#1297 = VECTOR('',#4707,1.) ;
#1298 = VECTOR('',#4710,1.00000000000064) ;
#1299 = VECTOR('',#4711,1.) ;
#1300 = VECTOR('',#4712,1.00000000000064) ;
#1301 = VECTOR('',#4713,1.) ;
#1302 = VECTOR('',#4714,1.00000000000064) ;
#1303 = VECTOR('',#4717,1.) ;
#1304 = VECTOR('',#4718,1.) ;
#1305 = VECTOR('',#4719,1.) ;
#1306 = VECTOR('',#4724,1.) ;
#1307 = VECTOR('',#4725,1.) ;
#1308 = VECTOR('',#4730,1.) ;
#1309 = VECTOR('',#4731,1.) ;
#1310 = VECTOR('',#4736,1.) ;
#1311 = VECTOR('',#4737,1.) ;
#1312 = VECTOR('',#4742,1.) ;
#1313 = VECTOR('',#4743,1.) ;
#1314 = VECTOR('',#4748,1.) ;
#1315 = VECTOR('',#4749,1.) ;
#1316 = VECTOR('',#4754,1.) ;
#1317 = VECTOR('',#4755,1.) ;
#1318 = VECTOR('',#4758,1.) ;
#1319 = VECTOR('',#4759,1.) ;
#1320 = VECTOR('',#4762,1.) ;
#1321 = VECTOR('',#4765,1.) ;
#1322 = VECTOR('',#4768,1.) ;
#1323 = VECTOR('',#4769,1.) ;
#1324 = VECTOR('',#4772,1.00000000000064) ;
#1325 = VECTOR('',#4775,1.00000000000064) ;
#1326 = VECTOR('',#4778,1.) ;
#1327 = VECTOR('',#4779,1.) ;
#1328 = VECTOR('',#4784,1.) ;
#1329 = VECTOR('',#4785,1.00000000000064) ;
#1330 = VECTOR('',#4788,1.) ;
#1331 = VECTOR('',#4793,1.) ;
#1332 = VECTOR('',#4794,1.00000000000064) ;
#1333 = VECTOR('',#4797,1.) ;
#1334 = VECTOR('',#4798,1.) ;
#1335 = VECTOR('',#4805,1.) ;
#1336 = VECTOR('',#4806,1.00000000000064) ;
#1337 = VECTOR('',#4809,1.) ;
#1338 = VECTOR('',#4814,1.00000000000064) ;
#1339 = VECTOR('',#4815,1.) ;
#1340 = VECTOR('',#4818,1.) ;
#1341 = VECTOR('',#4819,1.) ;
#1342 = VECTOR('',#4826,1.00000000000064) ;
#1343 = VECTOR('',#4827,1.) ;
#1344 = VECTOR('',#4830,1.) ;
#1345 = VECTOR('',#4835,1.) ;
#1346 = VECTOR('',#4836,1.) ;
#1347 = VECTOR('',#4839,1.) ;
#1348 = VECTOR('',#4844,1.00000000000064) ;
#1349 = VECTOR('',#4845,1.) ;
#1350 = VECTOR('',#4848,1.) ;
#1351 = VECTOR('',#4853,1.00000000000064) ;
#1352 = VECTOR('',#4854,1.) ;
#1353 = VECTOR('',#4857,1.) ;
#1354 = VECTOR('',#4858,1.) ;
#1355 = VECTOR('',#4865,1.) ;
#1356 = VECTOR('',#4866,1.00000000000064) ;
#1357 = VECTOR('',#4869,1.) ;
#1358 = VECTOR('',#4870,1.) ;
#1359 = VECTOR('',#4877,0.999999999999938) ;
#1360 = VECTOR('',#4878,1.00000000000032) ;
#1361 = VECTOR('',#4881,1.00000000000032) ;
#1362 = VECTOR('',#4884,1.00000000000064) ;
#1363 = VECTOR('',#4887,1.00000000000064) ;
#1364 = VECTOR('',#4890,1.00000000000032) ;
#1365 = VECTOR('',#4893,1.00000000000032) ;
#1366 = VECTOR('',#4896,1.00000000000064) ;
#1367 = VECTOR('',#4899,1.00000000000064) ;
#1368 = VECTOR('',#4902,1.00000000000032) ;
#1369 = VECTOR('',#4905,1.00000000000032) ;
#1370 = VECTOR('',#4908,0.999999999999935) ;
#1371 = VECTOR('',#4911,1.00000000000064) ;
#1372 = VECTOR('',#4914,0.999999999999855) ;
#1373 = VECTOR('',#4917,1.00000000000032) ;
#1374 = VECTOR('',#4920,1.00000000000064) ;
#1375 = VECTOR('',#4923,1.00000000000064) ;
#1376 = VECTOR('',#4926,1.00000000000032) ;
#1377 = VECTOR('',#4929,1.00000000000032) ;
#1378 = VECTOR('',#4932,1.00000000000064) ;
#1379 = VECTOR('',#4935,1.00000000000064) ;
#1380 = VECTOR('',#4938,1.00000000000032) ;
#1381 = VECTOR('',#4941,1.00000000000032) ;
#1382 = VECTOR('',#4944,1.00000000000064) ;
#1383 = VECTOR('',#4947,1.00000000000064) ;
#1384 = VECTOR('',#4950,1.00000000000032) ;
#1385 = VECTOR('',#4953,1.00000000000032) ;
#1386 = VECTOR('',#4956,1.00000000000064) ;
#1387 = VECTOR('',#4959,1.00000000000064) ;
#1388 = VECTOR('',#4962,1.00000000000032) ;
#1389 = VECTOR('',#4965,1.00000000000032) ;
#1390 = VECTOR('',#4968,1.00000000000064) ;
#1391 = VECTOR('',#4983,1.) ;
#1392 = VECTOR('',#4986,1.) ;
#1393 = VECTOR('',#4993,1.) ;
#1394 = VECTOR('',#4994,1.) ;
#1395 = VECTOR('',#4995,1.) ;
#1396 = VECTOR('',#4998,1.) ;
#1397 = VECTOR('',#5001,1.00000000000064) ;
#1398 = VECTOR('',#5004,1.) ;
#1399 = VECTOR('',#5007,1.00000000000064) ;
#1400 = VECTOR('',#5010,1.) ;
#1401 = VECTOR('',#5013,1.) ;
#1402 = VECTOR('',#5016,1.00000000000064) ;
#1403 = VECTOR('',#5019,1.00000000000064) ;
#1404 = VECTOR('',#5022,1.) ;
#1405 = VECTOR('',#5023,1.00000000000064) ;
#1406 = VECTOR('',#5028,1.00000000000032) ;
#1407 = VECTOR('',#5031,1.00000000000064) ;
#1408 = VECTOR('',#5032,1.00000000000032) ;
#1409 = VECTOR('',#5037,1.00000000000064) ;
#1410 = VECTOR('',#5040,1.) ;
#1411 = VECTOR('',#5041,1.00000000000064) ;
#1412 = VECTOR('',#5046,1.00000000000032) ;
#1413 = VECTOR('',#5049,1.00000000000064) ;
#1414 = VECTOR('',#5050,1.00000000000032) ;
#1415 = VECTOR('',#5055,1.00000000000064) ;
#1416 = VECTOR('',#5058,1.) ;
#1417 = VECTOR('',#5059,1.00000000000064) ;
#1418 = VECTOR('',#5064,1.00000000000064) ;
#1419 = VECTOR('',#5067,1.) ;
#1420 = VECTOR('',#5068,1.00000000000064) ;
#1421 = VECTOR('',#5071,1.00000000000064) ;
#1422 = VECTOR('',#5072,1.) ;
#1423 = VECTOR('',#5075,1.) ;
#1424 = VECTOR('',#5078,1.) ;
#1425 = VECTOR('',#5081,1.00000000000064) ;
#1426 = VECTOR('',#5084,1.) ;
#1427 = VECTOR('',#5087,1.00000000000064) ;
#1428 = VECTOR('',#5090,1.) ;
#1429 = VECTOR('',#5093,1.) ;
#1430 = VECTOR('',#5094,1.) ;
#1431 = VECTOR('',#5095,1.) ;
#1432 = VECTOR('',#5100,1.) ;
#1433 = VECTOR('',#5101,1.) ;
#1434 = VECTOR('',#5104,1.) ;
#1435 = VECTOR('',#5105,1.) ;
#1436 = VECTOR('',#5110,1.) ;
#1437 = VECTOR('',#5111,1.00000000000064) ;
#1438 = VECTOR('',#5114,1.00000000000064) ;
#1439 = VECTOR('',#5115,1.) ;
#1440 = VECTOR('',#5118,1.) ;
#1441 = VECTOR('',#5123,1.) ;
#1442 = VECTOR('',#5128,1.) ;
#1443 = VECTOR('',#5131,1.) ;
#1444 = VECTOR('',#5132,1.00000000000064) ;
#1445 = VECTOR('',#5139,1.) ;
#1446 = VECTOR('',#5140,1.00000000000064) ;
#1447 = VECTOR('',#5147,1.) ;
#1448 = VECTOR('',#5148,1.) ;
#1449 = VECTOR('',#5151,1.) ;
#1450 = VECTOR('',#5156,1.) ;
#1451 = VECTOR('',#5157,1.) ;
#1452 = VECTOR('',#5160,1.) ;
#1453 = VECTOR('',#5165,1.00000000000053) ;
#1454 = VECTOR('',#5166,1.00000000000064) ;
#1455 = VECTOR('',#5169,1.00000000000064) ;
#1456 = VECTOR('',#5170,1.) ;
#1457 = VECTOR('',#5173,1.00000000000032) ;
#1458 = VECTOR('',#5176,1.00000000000032) ;
#1459 = VECTOR('',#5179,1.00000000000064) ;
#1460 = VECTOR('',#5182,1.00000000000064) ;
#1461 = VECTOR('',#5185,1.00000000000032) ;
#1462 = VECTOR('',#5188,1.00000000000032) ;
#1463 = VECTOR('',#5191,1.00000000000064) ;
#1464 = VECTOR('',#5194,1.00000000000064) ;
#1465 = VECTOR('',#5195,1.) ;
#1466 = VECTOR('',#5198,1.0000000000003) ;
#1467 = VECTOR('',#5207,3.25) ;
#1468 = VECTOR('',#5212,1.) ;
#1469 = VECTOR('',#5219,3.25) ;
#1470 = VECTOR('',#5228,1.) ;
#1471 = VECTOR('',#5233,3.25) ;
#1472 = VECTOR('',#5238,1.) ;
#1473 = VECTOR('',#5245,3.25) ;
#1474 = VECTOR('',#5254,1.) ;
#1475 = VECTOR('',#5261,6.) ;
#1476 = VECTOR('',#5268,3.2) ;
#1477 = VECTOR('',#5281,6.) ;
#1478 = VECTOR('',#5288,3.2) ;
#1479 = VECTOR('',#5301,6.) ;
#1480 = VECTOR('',#5308,3.2) ;
#1481 = VECTOR('',#5321,6.) ;
#1482 = VECTOR('',#5328,3.2) ;
#1483 = VECTOR('',#5339,1.) ;
#1484 = VECTOR('',#5340,1.) ;
#1485 = VECTOR('',#5341,1.) ;
#1486 = VECTOR('',#5342,1.) ;
#1487 = VECTOR('',#5345,1.) ;
#1488 = VECTOR('',#5346,0.99999999999962) ;
#1489 = VECTOR('',#5347,0.99999999999962) ;
#1490 = VECTOR('',#5350,0.99999999999962) ;
#1491 = VECTOR('',#5351,1.) ;
#1492 = VECTOR('',#5352,0.99999999999962) ;
#1493 = VECTOR('',#5355,0.99999999999962) ;
#1494 = VECTOR('',#5356,1.) ;
#1495 = VECTOR('',#5357,0.99999999999962) ;
#1496 = VECTOR('',#5360,1.) ;
#1497 = VECTOR('',#5361,0.99999999999962) ;
#1498 = VECTOR('',#5364,0.99999999999962) ;
#1499 = VECTOR('',#5365,1.) ;
#1500 = VECTOR('',#5368,1.) ;
#1501 = VECTOR('',#5391,5.) ;
#1502 = VECTOR('',#5400,3.) ;
#1503 = VECTOR('',#5405,2.5) ;
#1504 = VECTOR('',#5410,1.) ;
#1505 = VECTOR('',#5411,1.) ;
#1506 = VECTOR('',#5412,1.) ;
#1507 = VECTOR('',#5413,1.) ;
#1508 = VECTOR('',#5416,1.) ;
#1509 = VECTOR('',#5417,0.99999999999962) ;
#1510 = VECTOR('',#5418,0.99999999999962) ;
#1511 = VECTOR('',#5421,0.99999999999962) ;
#1512 = VECTOR('',#5422,1.) ;
#1513 = VECTOR('',#5423,0.99999999999962) ;
#1514 = VECTOR('',#5426,0.99999999999962) ;
#1515 = VECTOR('',#5427,1.) ;
#1516 = VECTOR('',#5428,0.99999999999962) ;
#1517 = VECTOR('',#5431,1.) ;
#1518 = VECTOR('',#5432,0.99999999999962) ;
#1519 = VECTOR('',#5435,0.99999999999962) ;
#1520 = VECTOR('',#5436,1.) ;
#1521 = VECTOR('',#5439,1.) ;
#1522 = VECTOR('',#5462,5.) ;
#1523 = VECTOR('',#5471,3.) ;
#1524 = VECTOR('',#5476,2.5) ;
#1525 = VECTOR('',#5481,1.) ;
#1526 = VECTOR('',#5482,1.) ;
#1527 = VECTOR('',#5483,1.) ;
#1528 = VECTOR('',#5484,1.) ;
#1529 = VECTOR('',#5487,1.) ;
#1530 = VECTOR('',#5488,0.99999999999962) ;
#1531 = VECTOR('',#5489,0.99999999999962) ;
#1532 = VECTOR('',#5492,0.99999999999962) ;
#1533 = VECTOR('',#5493,1.) ;
#1534 = VECTOR('',#5494,0.99999999999962) ;
#1535 = VECTOR('',#5497,0.99999999999962) ;
#1536 = VECTOR('',#5498,1.) ;
#1537 = VECTOR('',#5499,0.99999999999962) ;
#1538 = VECTOR('',#5502,1.) ;
#1539 = VECTOR('',#5503,0.99999999999962) ;
#1540 = VECTOR('',#5506,0.99999999999962) ;
#1541 = VECTOR('',#5507,1.) ;
#1542 = VECTOR('',#5510,1.) ;
#1543 = VECTOR('',#5533,5.) ;
#1544 = VECTOR('',#5542,3.) ;
#1545 = VECTOR('',#5547,2.5) ;
#1546 = VECTOR('',#5552,1.) ;
#1547 = VECTOR('',#5553,1.) ;
#1548 = VECTOR('',#5554,1.) ;
#1549 = VECTOR('',#5555,1.) ;
#1550 = VECTOR('',#5558,1.) ;
#1551 = VECTOR('',#5559,0.99999999999962) ;
#1552 = VECTOR('',#5560,0.99999999999962) ;
#1553 = VECTOR('',#5563,0.99999999999962) ;
#1554 = VECTOR('',#5564,1.) ;
#1555 = VECTOR('',#5565,0.99999999999962) ;
#1556 = VECTOR('',#5568,0.99999999999962) ;
#1557 = VECTOR('',#5569,1.) ;
#1558 = VECTOR('',#5570,0.99999999999962) ;
#1559 = VECTOR('',#5573,1.) ;
#1560 = VECTOR('',#5574,0.99999999999962) ;
#1561 = VECTOR('',#5577,0.99999999999962) ;
#1562 = VECTOR('',#5578,1.) ;
#1563 = VECTOR('',#5581,1.) ;
#1564 = VECTOR('',#5604,5.) ;
#1565 = VECTOR('',#5613,3.) ;
#1566 = VECTOR('',#5618,2.5) ;
#1567 = CIRCLE('',#4019,27.5) ;
#1568 = CIRCLE('',#4020,27.5) ;
#1569 = CIRCLE('',#4022,28.5) ;
#1570 = CIRCLE('',#4024,28.5) ;
#1571 = CIRCLE('',#4026,3.25) ;
#1572 = CIRCLE('',#4027,3.25) ;
#1573 = CIRCLE('',#4029,3.85) ;
#1574 = CIRCLE('',#4031,3.25) ;
#1575 = CIRCLE('',#4032,3.25) ;
#1576 = CIRCLE('',#4034,3.85) ;
#1577 = CIRCLE('',#4036,3.25) ;
#1578 = CIRCLE('',#4037,3.25) ;
#1579 = CIRCLE('',#4039,3.85) ;
#1580 = CIRCLE('',#4041,3.25) ;
#1581 = CIRCLE('',#4042,3.25) ;
#1582 = CIRCLE('',#4044,3.85) ;
#1583 = CIRCLE('',#4046,1.39999840949753) ;
#1584 = CIRCLE('',#4047,1.39999840966918) ;
#1585 = CIRCLE('',#4048,1.39999840952888) ;
#1586 = CIRCLE('',#4049,1.39999901980282) ;
#1587 = CIRCLE('',#4050,1.39999901983735) ;
#1588 = CIRCLE('',#4051,1.39999901980293) ;
#1589 = CIRCLE('',#4053,0.8) ;
#1590 = CIRCLE('',#4056,0.6) ;
#1591 = CIRCLE('',#4059,0.6) ;
#1592 = CIRCLE('',#4062,0.6) ;
#1593 = CIRCLE('',#4065,0.6) ;
#1594 = CIRCLE('',#4068,0.8) ;
#1595 = CIRCLE('',#4071,0.8) ;
#1596 = CIRCLE('',#4074,0.6) ;
#1597 = CIRCLE('',#4077,0.6) ;
#1598 = CIRCLE('',#4080,0.8) ;
#1599 = CIRCLE('',#4083,0.8) ;
#1600 = CIRCLE('',#4086,0.6) ;
#1601 = CIRCLE('',#4089,0.6) ;
#1602 = CIRCLE('',#4092,0.6) ;
#1603 = CIRCLE('',#4095,0.6) ;
#1604 = CIRCLE('',#4098,0.8) ;
#1605 = CIRCLE('',#4102,1.39999901980304) ;
#1606 = CIRCLE('',#4103,1.39999901983726) ;
#1607 = CIRCLE('',#4104,1.39999901980286) ;
#1608 = CIRCLE('',#4105,1.39999840950088) ;
#1609 = CIRCLE('',#4106,1.39999840964119) ;
#1610 = CIRCLE('',#4107,1.39999840949753) ;
#1611 = CIRCLE('',#4109,0.8) ;
#1612 = CIRCLE('',#4111,0.8) ;
#1613 = CIRCLE('',#4113,0.8) ;
#1614 = CIRCLE('',#4115,0.8) ;
#1615 = CIRCLE('',#4117,0.8) ;
#1616 = CIRCLE('',#4119,0.8) ;
#1617 = CIRCLE('',#4127,0.6) ;
#1618 = CIRCLE('',#4130,0.6) ;
#1619 = CIRCLE('',#4134,0.6) ;
#1620 = CIRCLE('',#4137,0.6) ;
#1621 = CIRCLE('',#4141,0.6) ;
#1622 = CIRCLE('',#4144,0.6) ;
#1623 = CIRCLE('',#4147,0.6) ;
#1624 = CIRCLE('',#4150,0.6) ;
#1625 = CIRCLE('',#4154,0.6) ;
#1626 = CIRCLE('',#4158,0.6) ;
#1627 = CIRCLE('',#4194,27.5) ;
#1628 = CIRCLE('',#4195,28.5) ;
#1629 = CIRCLE('',#4197,27.5) ;
#1630 = CIRCLE('',#4199,28.5) ;
#1631 = CIRCLE('',#4201,0.03) ;
#1632 = CIRCLE('',#4202,1.6) ;
#1633 = CIRCLE('',#4203,0.4) ;
#1634 = CIRCLE('',#4204,0.4) ;
#1635 = CIRCLE('',#4205,1.6) ;
#1636 = CIRCLE('',#4206,0.03) ;
#1637 = CIRCLE('',#4208,0.63) ;
#1638 = CIRCLE('',#4211,1.) ;
#1639 = CIRCLE('',#4214,1.) ;
#1640 = CIRCLE('',#4217,1.) ;
#1641 = CIRCLE('',#4220,1.) ;
#1642 = CIRCLE('',#4223,0.63) ;
#1643 = CIRCLE('',#4227,0.03) ;
#1644 = CIRCLE('',#4228,1.6) ;
#1645 = CIRCLE('',#4229,0.4) ;
#1646 = CIRCLE('',#4230,0.4) ;
#1647 = CIRCLE('',#4231,1.6) ;
#1648 = CIRCLE('',#4232,0.03) ;
#1649 = CIRCLE('',#4234,1.) ;
#1650 = CIRCLE('',#4236,1.) ;
#1651 = CIRCLE('',#4240,1.) ;
#1652 = CIRCLE('',#4243,1.) ;
#1653 = CIRCLE('',#4245,3.25) ;
#1654 = CIRCLE('',#4246,3.25) ;
#1655 = CIRCLE('',#4248,3.25) ;
#1656 = CIRCLE('',#4249,3.25) ;
#1657 = CIRCLE('',#4252,0.63) ;
#1658 = CIRCLE('',#4255,0.63) ;
#1659 = CIRCLE('',#4270,3.25) ;
#1660 = CIRCLE('',#4271,3.25) ;
#1661 = CIRCLE('',#4273,3.75) ;
#1662 = CIRCLE('',#4275,3.25) ;
#1663 = CIRCLE('',#4276,3.25) ;
#1664 = CIRCLE('',#4278,3.75) ;
#1665 = CIRCLE('',#4281,3.25) ;
#1666 = CIRCLE('',#4282,3.25) ;
#1667 = CIRCLE('',#4284,3.75) ;
#1668 = CIRCLE('',#4286,3.25) ;
#1669 = CIRCLE('',#4287,3.25) ;
#1670 = CIRCLE('',#4289,3.75) ;
#1671 = CIRCLE('',#4293,6.) ;
#1672 = CIRCLE('',#4294,6.) ;
#1673 = CIRCLE('',#4296,3.2) ;
#1674 = CIRCLE('',#4297,3.2) ;
#1675 = CIRCLE('',#4302,6.) ;
#1676 = CIRCLE('',#4303,6.) ;
#1677 = CIRCLE('',#4305,3.2) ;
#1678 = CIRCLE('',#4306,3.2) ;
#1679 = CIRCLE('',#4311,6.) ;
#1680 = CIRCLE('',#4312,6.) ;
#1681 = CIRCLE('',#4314,3.2) ;
#1682 = CIRCLE('',#4315,3.2) ;
#1683 = CIRCLE('',#4320,6.) ;
#1684 = CIRCLE('',#4321,6.) ;
#1685 = CIRCLE('',#4323,3.2) ;
#1686 = CIRCLE('',#4324,3.2) ;
#1687 = CIRCLE('',#4336,4.4) ;
#1688 = CIRCLE('',#4338,5.) ;
#1689 = CIRCLE('',#4339,3.25) ;
#1690 = CIRCLE('',#4341,2.5) ;
#1691 = CIRCLE('',#4343,0.6) ;
#1692 = CIRCLE('',#4344,5.) ;
#1693 = CIRCLE('',#4347,0.25) ;
#1694 = CIRCLE('',#4348,3.) ;
#1695 = CIRCLE('',#4350,3.) ;
#1696 = CIRCLE('',#4361,4.4) ;
#1697 = CIRCLE('',#4363,5.) ;
#1698 = CIRCLE('',#4364,3.25) ;
#1699 = CIRCLE('',#4366,2.5) ;
#1700 = CIRCLE('',#4368,0.6) ;
#1701 = CIRCLE('',#4369,5.) ;
#1702 = CIRCLE('',#4372,0.25) ;
#1703 = CIRCLE('',#4373,3.) ;
#1704 = CIRCLE('',#4375,3.) ;
#1705 = CIRCLE('',#4386,4.4) ;
#1706 = CIRCLE('',#4388,5.) ;
#1707 = CIRCLE('',#4389,3.25) ;
#1708 = CIRCLE('',#4391,2.5) ;
#1709 = CIRCLE('',#4393,0.6) ;
#1710 = CIRCLE('',#4394,5.) ;
#1711 = CIRCLE('',#4397,0.25) ;
#1712 = CIRCLE('',#4398,3.) ;
#1713 = CIRCLE('',#4400,3.) ;
#1714 = CIRCLE('',#4411,4.4) ;
#1715 = CIRCLE('',#4413,5.) ;
#1716 = CIRCLE('',#4414,3.25) ;
#1717 = CIRCLE('',#4416,2.5) ;
#1718 = CIRCLE('',#4418,0.6) ;
#1719 = CIRCLE('',#4419,5.) ;
#1720 = CIRCLE('',#4422,0.25) ;
#1721 = CIRCLE('',#4423,3.) ;
#1722 = CIRCLE('',#4425,3.) ;
#1723 = VERTEX_POINT('',#5642) ;
#1724 = VERTEX_POINT('',#5643) ;
#1725 = VERTEX_POINT('',#5645) ;
#1726 = VERTEX_POINT('',#5647) ;
#1727 = VERTEX_POINT('',#5651) ;
#1728 = VERTEX_POINT('',#5655) ;
#1729 = VERTEX_POINT('',#5661) ;
#1730 = VERTEX_POINT('',#5662) ;
#1731 = VERTEX_POINT('',#5671) ;
#1732 = VERTEX_POINT('',#5673) ;
#1733 = VERTEX_POINT('',#5677) ;
#1734 = VERTEX_POINT('',#5681) ;
#1735 = VERTEX_POINT('',#5683) ;
#1736 = VERTEX_POINT('',#5687) ;
#1737 = VERTEX_POINT('',#5691) ;
#1738 = VERTEX_POINT('',#5693) ;
#1739 = VERTEX_POINT('',#5697) ;
#1740 = VERTEX_POINT('',#5701) ;
#1741 = VERTEX_POINT('',#5703) ;
#1742 = VERTEX_POINT('',#5707) ;
#1743 = VERTEX_POINT('',#5711) ;
#1744 = VERTEX_POINT('',#5713) ;
#1745 = VERTEX_POINT('',#5715) ;
#1746 = VERTEX_POINT('',#5717) ;
#1747 = VERTEX_POINT('',#5719) ;
#1748 = VERTEX_POINT('',#5721) ;
#1749 = VERTEX_POINT('',#5723) ;
#1750 = VERTEX_POINT('',#5725) ;
#1751 = VERTEX_POINT('',#5727) ;
#1752 = VERTEX_POINT('',#5729) ;
#1753 = VERTEX_POINT('',#5731) ;
#1754 = VERTEX_POINT('',#5733) ;
#1755 = VERTEX_POINT('',#5735) ;
#1756 = VERTEX_POINT('',#5737) ;
#1757 = VERTEX_POINT('',#5739) ;
#1758 = VERTEX_POINT('',#5741) ;
#1759 = VERTEX_POINT('',#5743) ;
#1760 = VERTEX_POINT('',#5745) ;
#1761 = VERTEX_POINT('',#5747) ;
#1762 = VERTEX_POINT('',#5749) ;
#1763 = VERTEX_POINT('',#5751) ;
#1764 = VERTEX_POINT('',#5753) ;
#1765 = VERTEX_POINT('',#5755) ;
#1766 = VERTEX_POINT('',#5757) ;
#1767 = VERTEX_POINT('',#5761) ;
#1768 = VERTEX_POINT('',#5763) ;
#1769 = VERTEX_POINT('',#5767) ;
#1770 = VERTEX_POINT('',#5771) ;
#1771 = VERTEX_POINT('',#5775) ;
#1772 = VERTEX_POINT('',#5779) ;
#1773 = VERTEX_POINT('',#5783) ;
#1774 = VERTEX_POINT('',#5787) ;
#1775 = VERTEX_POINT('',#5791) ;
#1776 = VERTEX_POINT('',#5795) ;
#1777 = VERTEX_POINT('',#5799) ;
#1778 = VERTEX_POINT('',#5803) ;
#1779 = VERTEX_POINT('',#5807) ;
#1780 = VERTEX_POINT('',#5811) ;
#1781 = VERTEX_POINT('',#5815) ;
#1782 = VERTEX_POINT('',#5819) ;
#1783 = VERTEX_POINT('',#5823) ;
#1784 = VERTEX_POINT('',#5827) ;
#1785 = VERTEX_POINT('',#5831) ;
#1786 = VERTEX_POINT('',#5835) ;
#1787 = VERTEX_POINT('',#5839) ;
#1788 = VERTEX_POINT('',#5843) ;
#1789 = VERTEX_POINT('',#5847) ;
#1790 = VERTEX_POINT('',#5851) ;
#1791 = VERTEX_POINT('',#5855) ;
#1792 = VERTEX_POINT('',#5859) ;
#1793 = VERTEX_POINT('',#5863) ;
#1794 = VERTEX_POINT('',#5867) ;
#1795 = VERTEX_POINT('',#5871) ;
#1796 = VERTEX_POINT('',#5875) ;
#1797 = VERTEX_POINT('',#5879) ;
#1798 = VERTEX_POINT('',#5883) ;
#1799 = VERTEX_POINT('',#5887) ;
#1800 = VERTEX_POINT('',#5891) ;
#1801 = VERTEX_POINT('',#5895) ;
#1802 = VERTEX_POINT('',#5896) ;
#1803 = VERTEX_POINT('',#5898) ;
#1804 = VERTEX_POINT('',#5900) ;
#1805 = VERTEX_POINT('',#5902) ;
#1806 = VERTEX_POINT('',#5904) ;
#1807 = VERTEX_POINT('',#5906) ;
#1808 = VERTEX_POINT('',#5908) ;
#1809 = VERTEX_POINT('',#5910) ;
#1810 = VERTEX_POINT('',#5912) ;
#1811 = VERTEX_POINT('',#5914) ;
#1812 = VERTEX_POINT('',#5916) ;
#1813 = VERTEX_POINT('',#5918) ;
#1814 = VERTEX_POINT('',#5920) ;
#1815 = VERTEX_POINT('',#5922) ;
#1816 = VERTEX_POINT('',#5924) ;
#1817 = VERTEX_POINT('',#5926) ;
#1818 = VERTEX_POINT('',#5928) ;
#1819 = VERTEX_POINT('',#5930) ;
#1820 = VERTEX_POINT('',#5932) ;
#1821 = VERTEX_POINT('',#5934) ;
#1822 = VERTEX_POINT('',#5936) ;
#1823 = VERTEX_POINT('',#5938) ;
#1824 = VERTEX_POINT('',#5940) ;
#1825 = VERTEX_POINT('',#5945) ;
#1826 = VERTEX_POINT('',#5946) ;
#1827 = VERTEX_POINT('',#5951) ;
#1828 = VERTEX_POINT('',#5952) ;
#1829 = VERTEX_POINT('',#5957) ;
#1830 = VERTEX_POINT('',#5958) ;
#1831 = VERTEX_POINT('',#5963) ;
#1832 = VERTEX_POINT('',#5964) ;
#1833 = VERTEX_POINT('',#5969) ;
#1834 = VERTEX_POINT('',#5970) ;
#1835 = VERTEX_POINT('',#5975) ;
#1836 = VERTEX_POINT('',#5976) ;
#1837 = VERTEX_POINT('',#5981) ;
#1838 = VERTEX_POINT('',#5989) ;
#1839 = VERTEX_POINT('',#5997) ;
#1840 = VERTEX_POINT('',#5999) ;
#1841 = VERTEX_POINT('',#6003) ;
#1842 = VERTEX_POINT('',#6007) ;
#1843 = VERTEX_POINT('',#6011) ;
#1844 = VERTEX_POINT('',#6015) ;
#1845 = VERTEX_POINT('',#6021) ;
#1846 = VERTEX_POINT('',#6025) ;
#1847 = VERTEX_POINT('',#6029) ;
#1848 = VERTEX_POINT('',#6033) ;
#1849 = VERTEX_POINT('',#6039) ;
#1850 = VERTEX_POINT('',#6043) ;
#1851 = VERTEX_POINT('',#6047) ;
#1852 = VERTEX_POINT('',#6051) ;
#1853 = VERTEX_POINT('',#6055) ;
#1854 = VERTEX_POINT('',#6059) ;
#1855 = VERTEX_POINT('',#6063) ;
#1856 = VERTEX_POINT('',#6067) ;
#1857 = VERTEX_POINT('',#6073) ;
#1858 = VERTEX_POINT('',#6077) ;
#1859 = VERTEX_POINT('',#6149) ;
#1860 = VERTEX_POINT('',#6150) ;
#1861 = VERTEX_POINT('',#6155) ;
#1862 = VERTEX_POINT('',#6157) ;
#1863 = VERTEX_POINT('',#6164) ;
#1864 = VERTEX_POINT('',#6166) ;
#1865 = VERTEX_POINT('',#6170) ;
#1866 = VERTEX_POINT('',#6171) ;
#1867 = VERTEX_POINT('',#6182) ;
#1868 = VERTEX_POINT('',#6184) ;
#1869 = VERTEX_POINT('',#6186) ;
#1870 = VERTEX_POINT('',#6188) ;
#1871 = VERTEX_POINT('',#6190) ;
#1872 = VERTEX_POINT('',#6192) ;
#1873 = VERTEX_POINT('',#6194) ;
#1874 = VERTEX_POINT('',#6196) ;
#1875 = VERTEX_POINT('',#6198) ;
#1876 = VERTEX_POINT('',#6200) ;
#1877 = VERTEX_POINT('',#6202) ;
#1878 = VERTEX_POINT('',#6204) ;
#1879 = VERTEX_POINT('',#6206) ;
#1880 = VERTEX_POINT('',#6208) ;
#1881 = VERTEX_POINT('',#6212) ;
#1882 = VERTEX_POINT('',#6214) ;
#1883 = VERTEX_POINT('',#6218) ;
#1884 = VERTEX_POINT('',#6222) ;
#1885 = VERTEX_POINT('',#6226) ;
#1886 = VERTEX_POINT('',#6230) ;
#1887 = VERTEX_POINT('',#6234) ;
#1888 = VERTEX_POINT('',#6238) ;
#1889 = VERTEX_POINT('',#6242) ;
#1890 = VERTEX_POINT('',#6246) ;
#1891 = VERTEX_POINT('',#6250) ;
#1892 = VERTEX_POINT('',#6254) ;
#1893 = VERTEX_POINT('',#6258) ;
#1894 = VERTEX_POINT('',#6262) ;
#1895 = VERTEX_POINT('',#6266) ;
#1896 = VERTEX_POINT('',#6267) ;
#1897 = VERTEX_POINT('',#6269) ;
#1898 = VERTEX_POINT('',#6271) ;
#1899 = VERTEX_POINT('',#6273) ;
#1900 = VERTEX_POINT('',#6275) ;
#1901 = VERTEX_POINT('',#6277) ;
#1902 = VERTEX_POINT('',#6279) ;
#1903 = VERTEX_POINT('',#6281) ;
#1904 = VERTEX_POINT('',#6283) ;
#1905 = VERTEX_POINT('',#6285) ;
#1906 = VERTEX_POINT('',#6287) ;
#1907 = VERTEX_POINT('',#6289) ;
#1908 = VERTEX_POINT('',#6291) ;
#1909 = VERTEX_POINT('',#6296) ;
#1910 = VERTEX_POINT('',#6297) ;
#1911 = VERTEX_POINT('',#6302) ;
#1912 = VERTEX_POINT('',#6304) ;
#1913 = VERTEX_POINT('',#6308) ;
#1914 = VERTEX_POINT('',#6312) ;
#1915 = VERTEX_POINT('',#6316) ;
#1916 = VERTEX_POINT('',#6322) ;
#1917 = VERTEX_POINT('',#6326) ;
#1918 = VERTEX_POINT('',#6329) ;
#1919 = VERTEX_POINT('',#6331) ;
#1920 = VERTEX_POINT('',#6334) ;
#1921 = VERTEX_POINT('',#6337) ;
#1922 = VERTEX_POINT('',#6339) ;
#1923 = VERTEX_POINT('',#6342) ;
#1924 = VERTEX_POINT('',#6346) ;
#1925 = VERTEX_POINT('',#6350) ;
#1926 = VERTEX_POINT('',#6354) ;
#1927 = VERTEX_POINT('',#6385) ;
#1928 = VERTEX_POINT('',#6386) ;
#1929 = VERTEX_POINT('',#6391) ;
#1930 = VERTEX_POINT('',#6395) ;
#1931 = VERTEX_POINT('',#6396) ;
#1932 = VERTEX_POINT('',#6401) ;
#1933 = VERTEX_POINT('',#6406) ;
#1934 = VERTEX_POINT('',#6407) ;
#1935 = VERTEX_POINT('',#6412) ;
#1936 = VERTEX_POINT('',#6416) ;
#1937 = VERTEX_POINT('',#6417) ;
#1938 = VERTEX_POINT('',#6422) ;
#1939 = VERTEX_POINT('',#6428) ;
#1940 = VERTEX_POINT('',#6430) ;
#1941 = VERTEX_POINT('',#6434) ;
#1942 = VERTEX_POINT('',#6436) ;
#1943 = VERTEX_POINT('',#6443) ;
#1944 = VERTEX_POINT('',#6445) ;
#1945 = VERTEX_POINT('',#6449) ;
#1946 = VERTEX_POINT('',#6451) ;
#1947 = VERTEX_POINT('',#6458) ;
#1948 = VERTEX_POINT('',#6460) ;
#1949 = VERTEX_POINT('',#6464) ;
#1950 = VERTEX_POINT('',#6466) ;
#1951 = VERTEX_POINT('',#6473) ;
#1952 = VERTEX_POINT('',#6475) ;
#1953 = VERTEX_POINT('',#6479) ;
#1954 = VERTEX_POINT('',#6481) ;
#1955 = VERTEX_POINT('',#6488) ;
#1956 = VERTEX_POINT('',#6489) ;
#1957 = VERTEX_POINT('',#6491) ;
#1958 = VERTEX_POINT('',#6493) ;
#1959 = VERTEX_POINT('',#6497) ;
#1960 = VERTEX_POINT('',#6498) ;
#1961 = VERTEX_POINT('',#6503) ;
#1962 = VERTEX_POINT('',#6505) ;
#1963 = VERTEX_POINT('',#6509) ;
#1964 = VERTEX_POINT('',#6511) ;
#1965 = VERTEX_POINT('',#6515) ;
#1966 = VERTEX_POINT('',#6519) ;
#1967 = VERTEX_POINT('',#6525) ;
#1968 = VERTEX_POINT('',#6528) ;
#1969 = VERTEX_POINT('',#6530) ;
#1970 = VERTEX_POINT('',#6533) ;
#1971 = VERTEX_POINT('',#6536) ;
#1972 = VERTEX_POINT('',#6542) ;
#1973 = VERTEX_POINT('',#6546) ;
#1974 = VERTEX_POINT('',#6553) ;
#1975 = VERTEX_POINT('',#6554) ;
#1976 = VERTEX_POINT('',#6556) ;
#1977 = VERTEX_POINT('',#6558) ;
#1978 = VERTEX_POINT('',#6562) ;
#1979 = VERTEX_POINT('',#6563) ;
#1980 = VERTEX_POINT('',#6568) ;
#1981 = VERTEX_POINT('',#6570) ;
#1982 = VERTEX_POINT('',#6574) ;
#1983 = VERTEX_POINT('',#6576) ;
#1984 = VERTEX_POINT('',#6580) ;
#1985 = VERTEX_POINT('',#6584) ;
#1986 = VERTEX_POINT('',#6590) ;
#1987 = VERTEX_POINT('',#6593) ;
#1988 = VERTEX_POINT('',#6595) ;
#1989 = VERTEX_POINT('',#6598) ;
#1990 = VERTEX_POINT('',#6601) ;
#1991 = VERTEX_POINT('',#6607) ;
#1992 = VERTEX_POINT('',#6611) ;
#1993 = VERTEX_POINT('',#6618) ;
#1994 = VERTEX_POINT('',#6619) ;
#1995 = VERTEX_POINT('',#6621) ;
#1996 = VERTEX_POINT('',#6623) ;
#1997 = VERTEX_POINT('',#6627) ;
#1998 = VERTEX_POINT('',#6628) ;
#1999 = VERTEX_POINT('',#6633) ;
#2000 = VERTEX_POINT('',#6635) ;
#2001 = VERTEX_POINT('',#6639) ;
#2002 = VERTEX_POINT('',#6641) ;
#2003 = VERTEX_POINT('',#6645) ;
#2004 = VERTEX_POINT('',#6649) ;
#2005 = VERTEX_POINT('',#6655) ;
#2006 = VERTEX_POINT('',#6658) ;
#2007 = VERTEX_POINT('',#6660) ;
#2008 = VERTEX_POINT('',#6663) ;
#2009 = VERTEX_POINT('',#6666) ;
#2010 = VERTEX_POINT('',#6672) ;
#2011 = VERTEX_POINT('',#6676) ;
#2012 = VERTEX_POINT('',#6683) ;
#2013 = VERTEX_POINT('',#6684) ;
#2014 = VERTEX_POINT('',#6686) ;
#2015 = VERTEX_POINT('',#6688) ;
#2016 = VERTEX_POINT('',#6692) ;
#2017 = VERTEX_POINT('',#6693) ;
#2018 = VERTEX_POINT('',#6698) ;
#2019 = VERTEX_POINT('',#6700) ;
#2020 = VERTEX_POINT('',#6704) ;
#2021 = VERTEX_POINT('',#6706) ;
#2022 = VERTEX_POINT('',#6710) ;
#2023 = VERTEX_POINT('',#6714) ;
#2024 = VERTEX_POINT('',#6720) ;
#2025 = VERTEX_POINT('',#6723) ;
#2026 = VERTEX_POINT('',#6725) ;
#2027 = VERTEX_POINT('',#6728) ;
#2028 = VERTEX_POINT('',#6731) ;
#2029 = VERTEX_POINT('',#6737) ;
#2030 = VERTEX_POINT('',#6741) ;
#2031 = EDGE_CURVE('',#1723,#1724,#1567,.F.) ;
#2032 = EDGE_CURVE('',#1724,#1725,#847,.T.) ;
#2033 = EDGE_CURVE('',#1726,#1725,#1568,.F.) ;
#2034 = EDGE_CURVE('',#1723,#1726,#848,.T.) ;
#2035 = EDGE_CURVE('',#1727,#1724,#263,.F.) ;
#2036 = EDGE_CURVE('',#1723,#1728,#264,.T.) ;
#2037 = EDGE_CURVE('',#1728,#1727,#1569,.F.) ;
#2038 = EDGE_CURVE('',#1729,#1730,#1570,.F.) ;
#2039 = EDGE_CURVE('',#1729,#1726,#265,.F.) ;
#2040 = EDGE_CURVE('',#1725,#1730,#266,.T.) ;
#2041 = EDGE_CURVE('',#1731,#1731,#1571,.F.) ;
#2042 = EDGE_CURVE('',#1731,#1732,#849,.T.) ;
#2043 = EDGE_CURVE('',#1732,#1732,#1572,.T.) ;
#2044 = EDGE_CURVE('',#1732,#1733,#850,.T.) ;
#2045 = EDGE_CURVE('',#1733,#1733,#1573,.T.) ;
#2046 = EDGE_CURVE('',#1734,#1734,#1574,.F.) ;
#2047 = EDGE_CURVE('',#1734,#1735,#851,.T.) ;
#2048 = EDGE_CURVE('',#1735,#1735,#1575,.T.) ;
#2049 = EDGE_CURVE('',#1735,#1736,#852,.T.) ;
#2050 = EDGE_CURVE('',#1736,#1736,#1576,.T.) ;
#2051 = EDGE_CURVE('',#1737,#1737,#1577,.F.) ;
#2052 = EDGE_CURVE('',#1737,#1738,#853,.T.) ;
#2053 = EDGE_CURVE('',#1738,#1738,#1578,.T.) ;
#2054 = EDGE_CURVE('',#1738,#1739,#854,.T.) ;
#2055 = EDGE_CURVE('',#1739,#1739,#1579,.T.) ;
#2056 = EDGE_CURVE('',#1740,#1740,#1580,.F.) ;
#2057 = EDGE_CURVE('',#1740,#1741,#855,.T.) ;
#2058 = EDGE_CURVE('',#1741,#1741,#1581,.T.) ;
#2059 = EDGE_CURVE('',#1741,#1742,#856,.T.) ;
#2060 = EDGE_CURVE('',#1742,#1742,#1582,.T.) ;
#2061 = EDGE_CURVE('',#1743,#1729,#857,.T.) ;
#2062 = EDGE_CURVE('',#1730,#1744,#858,.F.) ;
#2063 = EDGE_CURVE('',#1744,#1745,#859,.T.) ;
#2064 = EDGE_CURVE('',#1745,#1746,#1583,.T.) ;
#2065 = EDGE_CURVE('',#1746,#1747,#860,.T.) ;
#2066 = EDGE_CURVE('',#1747,#1748,#861,.T.) ;
#2067 = EDGE_CURVE('',#1748,#1749,#862,.F.) ;
#2068 = EDGE_CURVE('',#1749,#1750,#863,.F.) ;
#2069 = EDGE_CURVE('',#1750,#1751,#864,.F.) ;
#2070 = EDGE_CURVE('',#1751,#1752,#1584,.T.) ;
#2071 = EDGE_CURVE('',#1752,#1753,#865,.F.) ;
#2072 = EDGE_CURVE('',#1753,#1754,#1585,.T.) ;
#2073 = EDGE_CURVE('',#1754,#1755,#866,.F.) ;
#2074 = EDGE_CURVE('',#1755,#1756,#867,.F.) ;
#2075 = EDGE_CURVE('',#1756,#1757,#868,.T.) ;
#2076 = EDGE_CURVE('',#1757,#1758,#1586,.T.) ;
#2077 = EDGE_CURVE('',#1758,#1759,#869,.F.) ;
#2078 = EDGE_CURVE('',#1759,#1760,#1587,.T.) ;
#2079 = EDGE_CURVE('',#1760,#1761,#870,.T.) ;
#2080 = EDGE_CURVE('',#1761,#1762,#871,.F.) ;
#2081 = EDGE_CURVE('',#1762,#1763,#872,.T.) ;
#2082 = EDGE_CURVE('',#1763,#1764,#873,.F.) ;
#2083 = EDGE_CURVE('',#1764,#1765,#874,.F.) ;
#2084 = EDGE_CURVE('',#1765,#1766,#1588,.T.) ;
#2085 = EDGE_CURVE('',#1766,#1743,#875,.F.) ;
#2086 = EDGE_CURVE('',#1745,#1767,#876,.F.) ;
#2087 = EDGE_CURVE('',#1767,#1768,#1589,.T.) ;
#2088 = EDGE_CURVE('',#1746,#1768,#877,.F.) ;
#2089 = EDGE_CURVE('',#1768,#1769,#878,.T.) ;
#2090 = EDGE_CURVE('',#1747,#1769,#879,.F.) ;
#2091 = EDGE_CURVE('',#1769,#1770,#1590,.F.) ;
#2092 = EDGE_CURVE('',#1747,#1770,#880,.T.) ;
#2093 = EDGE_CURVE('',#1770,#1771,#881,.T.) ;
#2094 = EDGE_CURVE('',#1748,#1771,#882,.F.) ;
#2095 = EDGE_CURVE('',#1771,#1772,#1591,.F.) ;
#2096 = EDGE_CURVE('',#1748,#1772,#883,.T.) ;
#2097 = EDGE_CURVE('',#1772,#1773,#884,.F.) ;
#2098 = EDGE_CURVE('',#1749,#1773,#885,.F.) ;
#2099 = EDGE_CURVE('',#1773,#1774,#1592,.F.) ;
#2100 = EDGE_CURVE('',#1749,#1774,#886,.T.) ;
#2101 = EDGE_CURVE('',#1774,#1775,#887,.F.) ;
#2102 = EDGE_CURVE('',#1750,#1775,#888,.F.) ;
#2103 = EDGE_CURVE('',#1775,#1776,#1593,.F.) ;
#2104 = EDGE_CURVE('',#1750,#1776,#889,.T.) ;
#2105 = EDGE_CURVE('',#1776,#1777,#890,.F.) ;
#2106 = EDGE_CURVE('',#1751,#1777,#891,.F.) ;
#2107 = EDGE_CURVE('',#1777,#1778,#1594,.T.) ;
#2108 = EDGE_CURVE('',#1752,#1778,#892,.F.) ;
#2109 = EDGE_CURVE('',#1778,#1779,#893,.F.) ;
#2110 = EDGE_CURVE('',#1753,#1779,#894,.F.) ;
#2111 = EDGE_CURVE('',#1779,#1780,#1595,.T.) ;
#2112 = EDGE_CURVE('',#1754,#1780,#895,.F.) ;
#2113 = EDGE_CURVE('',#1780,#1781,#896,.F.) ;
#2114 = EDGE_CURVE('',#1755,#1781,#897,.F.) ;
#2115 = EDGE_CURVE('',#1781,#1782,#1596,.F.) ;
#2116 = EDGE_CURVE('',#1755,#1782,#898,.T.) ;
#2117 = EDGE_CURVE('',#1782,#1783,#899,.F.) ;
#2118 = EDGE_CURVE('',#1756,#1783,#900,.F.) ;
#2119 = EDGE_CURVE('',#1783,#1784,#1597,.F.) ;
#2120 = EDGE_CURVE('',#1756,#1784,#901,.T.) ;
#2121 = EDGE_CURVE('',#1784,#1785,#902,.T.) ;
#2122 = EDGE_CURVE('',#1757,#1785,#903,.F.) ;
#2123 = EDGE_CURVE('',#1785,#1786,#1598,.T.) ;
#2124 = EDGE_CURVE('',#1758,#1786,#904,.F.) ;
#2125 = EDGE_CURVE('',#1786,#1787,#905,.F.) ;
#2126 = EDGE_CURVE('',#1759,#1787,#906,.F.) ;
#2127 = EDGE_CURVE('',#1787,#1788,#1599,.T.) ;
#2128 = EDGE_CURVE('',#1760,#1788,#907,.F.) ;
#2129 = EDGE_CURVE('',#1788,#1789,#908,.T.) ;
#2130 = EDGE_CURVE('',#1761,#1789,#909,.F.) ;
#2131 = EDGE_CURVE('',#1789,#1790,#1600,.F.) ;
#2132 = EDGE_CURVE('',#1761,#1790,#910,.T.) ;
#2133 = EDGE_CURVE('',#1790,#1791,#911,.F.) ;
#2134 = EDGE_CURVE('',#1762,#1791,#912,.F.) ;
#2135 = EDGE_CURVE('',#1791,#1792,#1601,.F.) ;
#2136 = EDGE_CURVE('',#1762,#1792,#913,.T.) ;
#2137 = EDGE_CURVE('',#1792,#1793,#914,.T.) ;
#2138 = EDGE_CURVE('',#1763,#1793,#915,.F.) ;
#2139 = EDGE_CURVE('',#1793,#1794,#1602,.F.) ;
#2140 = EDGE_CURVE('',#1763,#1794,#916,.T.) ;
#2141 = EDGE_CURVE('',#1794,#1795,#917,.F.) ;
#2142 = EDGE_CURVE('',#1764,#1795,#918,.F.) ;
#2143 = EDGE_CURVE('',#1795,#1796,#1603,.F.) ;
#2144 = EDGE_CURVE('',#1764,#1796,#919,.T.) ;
#2145 = EDGE_CURVE('',#1796,#1797,#920,.F.) ;
#2146 = EDGE_CURVE('',#1765,#1797,#921,.F.) ;
#2147 = EDGE_CURVE('',#1797,#1798,#1604,.T.) ;
#2148 = EDGE_CURVE('',#1766,#1798,#922,.F.) ;
#2149 = EDGE_CURVE('',#1799,#1743,#923,.T.) ;
#2150 = EDGE_CURVE('',#1798,#1799,#924,.F.) ;
#2151 = EDGE_CURVE('',#1800,#1767,#925,.T.) ;
#2152 = EDGE_CURVE('',#1744,#1800,#926,.F.) ;
#2153 = EDGE_CURVE('',#1801,#1802,#927,.F.) ;
#2154 = EDGE_CURVE('',#1803,#1801,#1605,.T.) ;
#2155 = EDGE_CURVE('',#1804,#1803,#928,.F.) ;
#2156 = EDGE_CURVE('',#1805,#1804,#929,.F.) ;
#2157 = EDGE_CURVE('',#1806,#1805,#930,.T.) ;
#2158 = EDGE_CURVE('',#1807,#1806,#931,.F.) ;
#2159 = EDGE_CURVE('',#1808,#1807,#932,.T.) ;
#2160 = EDGE_CURVE('',#1809,#1808,#1606,.T.) ;
#2161 = EDGE_CURVE('',#1810,#1809,#933,.F.) ;
#2162 = EDGE_CURVE('',#1811,#1810,#1607,.T.) ;
#2163 = EDGE_CURVE('',#1812,#1811,#934,.T.) ;
#2164 = EDGE_CURVE('',#1813,#1812,#935,.F.) ;
#2165 = EDGE_CURVE('',#1814,#1813,#936,.F.) ;
#2166 = EDGE_CURVE('',#1815,#1814,#1608,.T.) ;
#2167 = EDGE_CURVE('',#1816,#1815,#937,.F.) ;
#2168 = EDGE_CURVE('',#1817,#1816,#1609,.T.) ;
#2169 = EDGE_CURVE('',#1818,#1817,#938,.F.) ;
#2170 = EDGE_CURVE('',#1819,#1818,#939,.F.) ;
#2171 = EDGE_CURVE('',#1820,#1819,#940,.F.) ;
#2172 = EDGE_CURVE('',#1821,#1820,#941,.T.) ;
#2173 = EDGE_CURVE('',#1822,#1821,#942,.T.) ;
#2174 = EDGE_CURVE('',#1823,#1822,#1610,.T.) ;
#2175 = EDGE_CURVE('',#1824,#1823,#943,.T.) ;
#2176 = EDGE_CURVE('',#1727,#1824,#944,.F.) ;
#2177 = EDGE_CURVE('',#1802,#1728,#945,.T.) ;
#2178 = EDGE_CURVE('',#1825,#1826,#1611,.F.) ;
#2179 = EDGE_CURVE('',#1778,#1826,#946,.F.) ;
#2180 = EDGE_CURVE('',#1777,#1825,#947,.F.) ;
#2181 = EDGE_CURVE('',#1827,#1828,#1612,.F.) ;
#2182 = EDGE_CURVE('',#1780,#1828,#948,.F.) ;
#2183 = EDGE_CURVE('',#1779,#1827,#949,.F.) ;
#2184 = EDGE_CURVE('',#1829,#1830,#1613,.F.) ;
#2185 = EDGE_CURVE('',#1786,#1830,#950,.F.) ;
#2186 = EDGE_CURVE('',#1785,#1829,#951,.F.) ;
#2187 = EDGE_CURVE('',#1831,#1832,#1614,.F.) ;
#2188 = EDGE_CURVE('',#1788,#1832,#952,.F.) ;
#2189 = EDGE_CURVE('',#1787,#1831,#953,.F.) ;
#2190 = EDGE_CURVE('',#1833,#1834,#1615,.F.) ;
#2191 = EDGE_CURVE('',#1798,#1834,#954,.F.) ;
#2192 = EDGE_CURVE('',#1797,#1833,#955,.F.) ;
#2193 = EDGE_CURVE('',#1835,#1836,#1616,.F.) ;
#2194 = EDGE_CURVE('',#1768,#1836,#956,.F.) ;
#2195 = EDGE_CURVE('',#1767,#1835,#957,.F.) ;
#2196 = EDGE_CURVE('',#1837,#1835,#958,.T.) ;
#2197 = EDGE_CURVE('',#1837,#1800,#959,.T.) ;
#2198 = EDGE_CURVE('',#1830,#1831,#960,.F.) ;
#2199 = EDGE_CURVE('',#1826,#1827,#961,.F.) ;
#2200 = EDGE_CURVE('',#1838,#1799,#962,.T.) ;
#2201 = EDGE_CURVE('',#1834,#1838,#963,.F.) ;
#2202 = EDGE_CURVE('',#1837,#1824,#964,.T.) ;
#2203 = EDGE_CURVE('',#1802,#1838,#965,.F.) ;
#2204 = EDGE_CURVE('',#1839,#1772,#966,.T.) ;
#2205 = EDGE_CURVE('',#1840,#1771,#967,.T.) ;
#2206 = EDGE_CURVE('',#1840,#1839,#1617,.T.) ;
#2207 = EDGE_CURVE('',#1841,#1773,#968,.T.) ;
#2208 = EDGE_CURVE('',#1839,#1841,#969,.F.) ;
#2209 = EDGE_CURVE('',#1842,#1774,#970,.T.) ;
#2210 = EDGE_CURVE('',#1841,#1842,#1618,.T.) ;
#2211 = EDGE_CURVE('',#1843,#1776,#971,.T.) ;
#2212 = EDGE_CURVE('',#1843,#1825,#972,.F.) ;
#2213 = EDGE_CURVE('',#1844,#1775,#973,.T.) ;
#2214 = EDGE_CURVE('',#1842,#1844,#974,.F.) ;
#2215 = EDGE_CURVE('',#1844,#1843,#1619,.T.) ;
#2216 = EDGE_CURVE('',#1845,#1781,#975,.T.) ;
#2217 = EDGE_CURVE('',#1828,#1845,#976,.F.) ;
#2218 = EDGE_CURVE('',#1846,#1782,#977,.T.) ;
#2219 = EDGE_CURVE('',#1845,#1846,#1620,.T.) ;
#2220 = EDGE_CURVE('',#1847,#1829,#978,.T.) ;
#2221 = EDGE_CURVE('',#1847,#1784,#979,.T.) ;
#2222 = EDGE_CURVE('',#1848,#1783,#980,.T.) ;
#2223 = EDGE_CURVE('',#1846,#1848,#981,.F.) ;
#2224 = EDGE_CURVE('',#1848,#1847,#1621,.T.) ;
#2225 = EDGE_CURVE('',#1832,#1849,#982,.T.) ;
#2226 = EDGE_CURVE('',#1849,#1789,#983,.T.) ;
#2227 = EDGE_CURVE('',#1850,#1790,#984,.T.) ;
#2228 = EDGE_CURVE('',#1849,#1850,#1622,.T.) ;
#2229 = EDGE_CURVE('',#1851,#1791,#985,.T.) ;
#2230 = EDGE_CURVE('',#1850,#1851,#986,.F.) ;
#2231 = EDGE_CURVE('',#1852,#1792,#987,.T.) ;
#2232 = EDGE_CURVE('',#1851,#1852,#1623,.T.) ;
#2233 = EDGE_CURVE('',#1852,#1853,#988,.T.) ;
#2234 = EDGE_CURVE('',#1853,#1793,#989,.T.) ;
#2235 = EDGE_CURVE('',#1854,#1794,#990,.T.) ;
#2236 = EDGE_CURVE('',#1853,#1854,#1624,.T.) ;
#2237 = EDGE_CURVE('',#1836,#1855,#991,.T.) ;
#2238 = EDGE_CURVE('',#1855,#1769,#992,.T.) ;
#2239 = EDGE_CURVE('',#1856,#1840,#993,.T.) ;
#2240 = EDGE_CURVE('',#1856,#1770,#994,.T.) ;
#2241 = EDGE_CURVE('',#1855,#1856,#1625,.T.) ;
#2242 = EDGE_CURVE('',#1857,#1796,#995,.T.) ;
#2243 = EDGE_CURVE('',#1857,#1833,#996,.F.) ;
#2244 = EDGE_CURVE('',#1858,#1795,#997,.T.) ;
#2245 = EDGE_CURVE('',#1854,#1858,#998,.F.) ;
#2246 = EDGE_CURVE('',#1858,#1857,#1626,.T.) ;
#2247 = EDGE_CURVE('',#1835,#1823,#999,.T.) ;
#2248 = EDGE_CURVE('',#1836,#1822,#1000,.T.) ;
#2249 = EDGE_CURVE('',#1855,#1821,#1001,.T.) ;
#2250 = EDGE_CURVE('',#1856,#1821,#1002,.F.) ;
#2251 = EDGE_CURVE('',#1840,#1820,#1003,.T.) ;
#2252 = EDGE_CURVE('',#1839,#1820,#1004,.F.) ;
#2253 = EDGE_CURVE('',#1841,#1819,#1005,.T.) ;
#2254 = EDGE_CURVE('',#1842,#1819,#1006,.F.) ;
#2255 = EDGE_CURVE('',#1844,#1818,#1007,.T.) ;
#2256 = EDGE_CURVE('',#1843,#1818,#1008,.F.) ;
#2257 = EDGE_CURVE('',#1825,#1817,#1009,.T.) ;
#2258 = EDGE_CURVE('',#1826,#1816,#1010,.T.) ;
#2259 = EDGE_CURVE('',#1827,#1815,#1011,.T.) ;
#2260 = EDGE_CURVE('',#1828,#1814,#1012,.T.) ;
#2261 = EDGE_CURVE('',#1845,#1813,#1013,.T.) ;
#2262 = EDGE_CURVE('',#1846,#1813,#1014,.F.) ;
#2263 = EDGE_CURVE('',#1848,#1812,#1015,.T.) ;
#2264 = EDGE_CURVE('',#1847,#1812,#1016,.F.) ;
#2265 = EDGE_CURVE('',#1829,#1811,#1017,.T.) ;
#2266 = EDGE_CURVE('',#1830,#1810,#1018,.T.) ;
#2267 = EDGE_CURVE('',#1831,#1809,#1019,.T.) ;
#2268 = EDGE_CURVE('',#1832,#1808,#1020,.T.) ;
#2269 = EDGE_CURVE('',#1849,#1807,#1021,.T.) ;
#2270 = EDGE_CURVE('',#1850,#1807,#1022,.F.) ;
#2271 = EDGE_CURVE('',#1851,#1806,#1023,.T.) ;
#2272 = EDGE_CURVE('',#1852,#1806,#1024,.F.) ;
#2273 = EDGE_CURVE('',#1853,#1805,#1025,.T.) ;
#2274 = EDGE_CURVE('',#1854,#1805,#1026,.F.) ;
#2275 = EDGE_CURVE('',#1858,#1804,#1027,.T.) ;
#2276 = EDGE_CURVE('',#1857,#1804,#1028,.F.) ;
#2277 = EDGE_CURVE('',#1833,#1803,#1029,.T.) ;
#2278 = EDGE_CURVE('',#1834,#1801,#1030,.T.) ;
#2279 = EDGE_CURVE('',#1859,#1860,#59,.F.) ;
#2280 = EDGE_CURVE('',#1861,#1860,#1627,.F.) ;
#2281 = EDGE_CURVE('',#1861,#1862,#60,.T.) ;
#2282 = EDGE_CURVE('',#1862,#1859,#1628,.F.) ;
#2283 = EDGE_CURVE('',#1860,#1863,#1031,.T.) ;
#2284 = EDGE_CURVE('',#1864,#1863,#1629,.F.) ;
#2285 = EDGE_CURVE('',#1861,#1864,#1032,.T.) ;
#2286 = EDGE_CURVE('',#1865,#1866,#1630,.F.) ;
#2287 = EDGE_CURVE('',#1865,#1864,#61,.F.) ;
#2288 = EDGE_CURVE('',#1863,#1866,#62,.T.) ;
#2289 = EDGE_CURVE('',#1867,#1865,#1033,.F.) ;
#2290 = EDGE_CURVE('',#1866,#1868,#1034,.T.) ;
#2291 = EDGE_CURVE('',#1868,#1869,#1035,.F.) ;
#2292 = EDGE_CURVE('',#1869,#1870,#1631,.T.) ;
#2293 = EDGE_CURVE('',#1870,#1871,#1036,.F.) ;
#2294 = EDGE_CURVE('',#1871,#1872,#1632,.F.) ;
#2295 = EDGE_CURVE('',#1872,#1873,#1037,.F.) ;
#2296 = EDGE_CURVE('',#1873,#1874,#1633,.T.) ;
#2297 = EDGE_CURVE('',#1874,#1875,#1038,.F.) ;
#2298 = EDGE_CURVE('',#1875,#1876,#1634,.T.) ;
#2299 = EDGE_CURVE('',#1876,#1877,#1039,.T.) ;
#2300 = EDGE_CURVE('',#1877,#1878,#1635,.F.) ;
#2301 = EDGE_CURVE('',#1878,#1879,#1040,.F.) ;
#2302 = EDGE_CURVE('',#1879,#1880,#1636,.T.) ;
#2303 = EDGE_CURVE('',#1880,#1867,#1041,.T.) ;
#2304 = EDGE_CURVE('',#1869,#1881,#1042,.T.) ;
#2305 = EDGE_CURVE('',#1881,#1882,#1637,.T.) ;
#2306 = EDGE_CURVE('',#1870,#1882,#1043,.T.) ;
#2307 = EDGE_CURVE('',#1882,#1883,#1044,.F.) ;
#2308 = EDGE_CURVE('',#1871,#1883,#1045,.F.) ;
#2309 = EDGE_CURVE('',#1883,#1884,#1638,.F.) ;
#2310 = EDGE_CURVE('',#1872,#1884,#1046,.F.) ;
#2311 = EDGE_CURVE('',#1884,#1885,#1047,.F.) ;
#2312 = EDGE_CURVE('',#1873,#1885,#1048,.F.) ;
#2313 = EDGE_CURVE('',#1885,#1886,#1639,.T.) ;
#2314 = EDGE_CURVE('',#1874,#1886,#1049,.T.) ;
#2315 = EDGE_CURVE('',#1886,#1887,#1050,.F.) ;
#2316 = EDGE_CURVE('',#1875,#1887,#1051,.F.) ;
#2317 = EDGE_CURVE('',#1887,#1888,#1640,.T.) ;
#2318 = EDGE_CURVE('',#1876,#1888,#1052,.T.) ;
#2319 = EDGE_CURVE('',#1888,#1889,#1053,.T.) ;
#2320 = EDGE_CURVE('',#1877,#1889,#1054,.F.) ;
#2321 = EDGE_CURVE('',#1889,#1890,#1641,.F.) ;
#2322 = EDGE_CURVE('',#1878,#1890,#1055,.F.) ;
#2323 = EDGE_CURVE('',#1890,#1891,#1056,.F.) ;
#2324 = EDGE_CURVE('',#1879,#1891,#1057,.F.) ;
#2325 = EDGE_CURVE('',#1891,#1892,#1642,.T.) ;
#2326 = EDGE_CURVE('',#1880,#1892,#1058,.T.) ;
#2327 = EDGE_CURVE('',#1892,#1893,#1059,.T.) ;
#2328 = EDGE_CURVE('',#1893,#1867,#1060,.T.) ;
#2329 = EDGE_CURVE('',#1868,#1894,#1061,.F.) ;
#2330 = EDGE_CURVE('',#1894,#1881,#1062,.F.) ;
#2331 = EDGE_CURVE('',#1895,#1896,#1063,.T.) ;
#2332 = EDGE_CURVE('',#1897,#1895,#1643,.T.) ;
#2333 = EDGE_CURVE('',#1898,#1897,#1064,.F.) ;
#2334 = EDGE_CURVE('',#1899,#1898,#1644,.F.) ;
#2335 = EDGE_CURVE('',#1900,#1899,#1065,.T.) ;
#2336 = EDGE_CURVE('',#1901,#1900,#1645,.T.) ;
#2337 = EDGE_CURVE('',#1902,#1901,#1066,.F.) ;
#2338 = EDGE_CURVE('',#1903,#1902,#1646,.T.) ;
#2339 = EDGE_CURVE('',#1904,#1903,#1067,.F.) ;
#2340 = EDGE_CURVE('',#1905,#1904,#1647,.F.) ;
#2341 = EDGE_CURVE('',#1906,#1905,#1068,.F.) ;
#2342 = EDGE_CURVE('',#1907,#1906,#1648,.T.) ;
#2343 = EDGE_CURVE('',#1908,#1907,#1069,.F.) ;
#2344 = EDGE_CURVE('',#1859,#1908,#1070,.T.) ;
#2345 = EDGE_CURVE('',#1896,#1862,#1071,.F.) ;
#2346 = EDGE_CURVE('',#1909,#1910,#1649,.F.) ;
#2347 = EDGE_CURVE('',#1890,#1910,#1072,.F.) ;
#2348 = EDGE_CURVE('',#1889,#1909,#1073,.F.) ;
#2349 = EDGE_CURVE('',#1911,#1886,#1074,.T.) ;
#2350 = EDGE_CURVE('',#1912,#1885,#1075,.T.) ;
#2351 = EDGE_CURVE('',#1912,#1911,#1650,.T.) ;
#2352 = EDGE_CURVE('',#1884,#1913,#1076,.F.) ;
#2353 = EDGE_CURVE('',#1913,#1912,#1077,.F.) ;
#2354 = EDGE_CURVE('',#1914,#1909,#1078,.T.) ;
#2355 = EDGE_CURVE('',#1914,#1888,#1079,.T.) ;
#2356 = EDGE_CURVE('',#1915,#1887,#1080,.T.) ;
#2357 = EDGE_CURVE('',#1915,#1914,#1651,.T.) ;
#2358 = EDGE_CURVE('',#1911,#1915,#1081,.F.) ;
#2359 = EDGE_CURVE('',#1916,#1913,#1652,.F.) ;
#2360 = EDGE_CURVE('',#1883,#1916,#1082,.F.) ;
#2361 = EDGE_CURVE('',#1917,#1893,#1083,.T.) ;
#2362 = EDGE_CURVE('',#1896,#1917,#1084,.F.) ;
#2363 = EDGE_CURVE('',#1918,#1918,#1653,.T.) ;
#2364 = EDGE_CURVE('',#1919,#1919,#1654,.T.) ;
#2365 = EDGE_CURVE('',#1920,#1894,#1085,.T.) ;
#2366 = EDGE_CURVE('',#1920,#1908,#1086,.T.) ;
#2367 = EDGE_CURVE('',#1921,#1921,#1655,.T.) ;
#2368 = EDGE_CURVE('',#1922,#1922,#1656,.T.) ;
#2369 = EDGE_CURVE('',#1923,#1917,#1087,.T.) ;
#2370 = EDGE_CURVE('',#1923,#1892,#1088,.T.) ;
#2371 = EDGE_CURVE('',#1924,#1891,#1089,.T.) ;
#2372 = EDGE_CURVE('',#1924,#1923,#1657,.T.) ;
#2373 = EDGE_CURVE('',#1925,#1881,#1090,.T.) ;
#2374 = EDGE_CURVE('',#1920,#1925,#1091,.F.) ;
#2375 = EDGE_CURVE('',#1926,#1882,#1092,.T.) ;
#2376 = EDGE_CURVE('',#1925,#1926,#1658,.T.) ;
#2377 = EDGE_CURVE('',#1925,#1907,#1093,.F.) ;
#2378 = EDGE_CURVE('',#1926,#1906,#1094,.F.) ;
#2379 = EDGE_CURVE('',#1916,#1905,#1095,.T.) ;
#2380 = EDGE_CURVE('',#1926,#1916,#1096,.F.) ;
#2381 = EDGE_CURVE('',#1913,#1904,#1097,.T.) ;
#2382 = EDGE_CURVE('',#1912,#1903,#1098,.T.) ;
#2383 = EDGE_CURVE('',#1911,#1902,#1099,.F.) ;
#2384 = EDGE_CURVE('',#1915,#1901,#1100,.T.) ;
#2385 = EDGE_CURVE('',#1914,#1900,#1101,.F.) ;
#2386 = EDGE_CURVE('',#1909,#1899,#1102,.T.) ;
#2387 = EDGE_CURVE('',#1910,#1898,#1103,.T.) ;
#2388 = EDGE_CURVE('',#1924,#1897,#1104,.T.) ;
#2389 = EDGE_CURVE('',#1910,#1924,#1105,.F.) ;
#2390 = EDGE_CURVE('',#1923,#1895,#1106,.F.) ;
#2391 = EDGE_CURVE('',#1927,#1928,#1659,.F.) ;
#2392 = EDGE_CURVE('',#1928,#1922,#1107,.T.) ;
#2393 = EDGE_CURVE('',#1928,#1927,#1660,.F.) ;
#2394 = EDGE_CURVE('',#1927,#1929,#1108,.T.) ;
#2395 = EDGE_CURVE('',#1929,#1929,#1661,.T.) ;
#2396 = EDGE_CURVE('',#1930,#1931,#1662,.F.) ;
#2397 = EDGE_CURVE('',#1931,#1921,#1109,.T.) ;
#2398 = EDGE_CURVE('',#1931,#1930,#1663,.F.) ;
#2399 = EDGE_CURVE('',#1932,#1932,#1664,.T.) ;
#2400 = EDGE_CURVE('',#1930,#1932,#1110,.T.) ;
#2401 = EDGE_CURVE('',#1933,#1934,#1665,.F.) ;
#2402 = EDGE_CURVE('',#1934,#1919,#1111,.T.) ;
#2403 = EDGE_CURVE('',#1934,#1933,#1666,.F.) ;
#2404 = EDGE_CURVE('',#1933,#1935,#1112,.T.) ;
#2405 = EDGE_CURVE('',#1935,#1935,#1667,.T.) ;
#2406 = EDGE_CURVE('',#1936,#1937,#1668,.F.) ;
#2407 = EDGE_CURVE('',#1937,#1918,#1113,.T.) ;
#2408 = EDGE_CURVE('',#1937,#1936,#1669,.F.) ;
#2409 = EDGE_CURVE('',#1938,#1938,#1670,.T.) ;
#2410 = EDGE_CURVE('',#1936,#1938,#1114,.T.) ;
#2411 = EDGE_CURVE('',#1939,#1939,#1671,.T.) ;
#2412 = EDGE_CURVE('',#1939,#1940,#1115,.T.) ;
#2413 = EDGE_CURVE('',#1940,#1940,#1672,.T.) ;
#2414 = EDGE_CURVE('',#1941,#1941,#1673,.T.) ;
#2415 = EDGE_CURVE('',#1941,#1942,#1116,.T.) ;
#2416 = EDGE_CURVE('',#1942,#1942,#1674,.T.) ;
#2417 = EDGE_CURVE('',#1943,#1943,#1675,.T.) ;
#2418 = EDGE_CURVE('',#1943,#1944,#1117,.T.) ;
#2419 = EDGE_CURVE('',#1944,#1944,#1676,.T.) ;
#2420 = EDGE_CURVE('',#1945,#1945,#1677,.T.) ;
#2421 = EDGE_CURVE('',#1945,#1946,#1118,.T.) ;
#2422 = EDGE_CURVE('',#1946,#1946,#1678,.T.) ;
#2423 = EDGE_CURVE('',#1947,#1947,#1679,.T.) ;
#2424 = EDGE_CURVE('',#1947,#1948,#1119,.T.) ;
#2425 = EDGE_CURVE('',#1948,#1948,#1680,.T.) ;
#2426 = EDGE_CURVE('',#1949,#1949,#1681,.T.) ;
#2427 = EDGE_CURVE('',#1949,#1950,#1120,.T.) ;
#2428 = EDGE_CURVE('',#1950,#1950,#1682,.T.) ;
#2429 = EDGE_CURVE('',#1951,#1951,#1683,.T.) ;
#2430 = EDGE_CURVE('',#1951,#1952,#1121,.T.) ;
#2431 = EDGE_CURVE('',#1952,#1952,#1684,.T.) ;
#2432 = EDGE_CURVE('',#1953,#1953,#1685,.T.) ;
#2433 = EDGE_CURVE('',#1953,#1954,#1122,.T.) ;
#2434 = EDGE_CURVE('',#1954,#1954,#1686,.T.) ;
#2435 = EDGE_CURVE('',#1955,#1956,#1123,.T.) ;
#2436 = EDGE_CURVE('',#1955,#1957,#1124,.T.) ;
#2437 = EDGE_CURVE('',#1957,#1958,#1125,.T.) ;
#2438 = EDGE_CURVE('',#1956,#1958,#1126,.T.) ;
#2439 = EDGE_CURVE('',#1959,#1960,#1127,.T.) ;
#2440 = EDGE_CURVE('',#1959,#1955,#1128,.T.) ;
#2441 = EDGE_CURVE('',#1960,#1956,#1129,.T.) ;
#2442 = EDGE_CURVE('',#1957,#1961,#1130,.T.) ;
#2443 = EDGE_CURVE('',#1961,#1962,#1131,.T.) ;
#2444 = EDGE_CURVE('',#1958,#1962,#1132,.T.) ;
#2445 = EDGE_CURVE('',#1962,#1963,#1133,.T.) ;
#2446 = EDGE_CURVE('',#1963,#1964,#1134,.T.) ;
#2447 = EDGE_CURVE('',#1964,#1960,#1135,.T.) ;
#2448 = EDGE_CURVE('',#1965,#1964,#1136,.T.) ;
#2449 = EDGE_CURVE('',#1965,#1959,#1137,.T.) ;
#2450 = EDGE_CURVE('',#1961,#1966,#1138,.T.) ;
#2451 = EDGE_CURVE('',#1966,#1963,#1139,.T.) ;
#2452 = EDGE_CURVE('',#1966,#1965,#1140,.T.) ;
#2453 = EDGE_CURVE('',#1967,#1967,#1687,.T.) ;
#2454 = EDGE_CURVE('',#1968,#1968,#1688,.T.) ;
#2455 = EDGE_CURVE('',#1969,#1969,#1689,.T.) ;
#2456 = EDGE_CURVE('',#1970,#1970,#1690,.T.) ;
#2457 = EDGE_CURVE('',#1967,#1971,#1691,.T.) ;
#2458 = EDGE_CURVE('',#1971,#1971,#1692,.T.) ;
#2459 = EDGE_CURVE('',#1971,#1968,#1141,.T.) ;
#2460 = EDGE_CURVE('',#1969,#1972,#1693,.T.) ;
#2461 = EDGE_CURVE('',#1972,#1972,#1694,.T.) ;
#2462 = EDGE_CURVE('',#1972,#1973,#1142,.T.) ;
#2463 = EDGE_CURVE('',#1973,#1973,#1695,.T.) ;
#2464 = EDGE_CURVE('',#1973,#1970,#1143,.T.) ;
#2465 = EDGE_CURVE('',#1974,#1975,#1144,.T.) ;
#2466 = EDGE_CURVE('',#1974,#1976,#1145,.T.) ;
#2467 = EDGE_CURVE('',#1976,#1977,#1146,.T.) ;
#2468 = EDGE_CURVE('',#1975,#1977,#1147,.T.) ;
#2469 = EDGE_CURVE('',#1978,#1979,#1148,.T.) ;
#2470 = EDGE_CURVE('',#1978,#1974,#1149,.T.) ;
#2471 = EDGE_CURVE('',#1979,#1975,#1150,.T.) ;
#2472 = EDGE_CURVE('',#1976,#1980,#1151,.T.) ;
#2473 = EDGE_CURVE('',#1980,#1981,#1152,.T.) ;
#2474 = EDGE_CURVE('',#1977,#1981,#1153,.T.) ;
#2475 = EDGE_CURVE('',#1981,#1982,#1154,.T.) ;
#2476 = EDGE_CURVE('',#1982,#1983,#1155,.T.) ;
#2477 = EDGE_CURVE('',#1983,#1979,#1156,.T.) ;
#2478 = EDGE_CURVE('',#1984,#1983,#1157,.T.) ;
#2479 = EDGE_CURVE('',#1984,#1978,#1158,.T.) ;
#2480 = EDGE_CURVE('',#1980,#1985,#1159,.T.) ;
#2481 = EDGE_CURVE('',#1985,#1982,#1160,.T.) ;
#2482 = EDGE_CURVE('',#1985,#1984,#1161,.T.) ;
#2483 = EDGE_CURVE('',#1986,#1986,#1696,.T.) ;
#2484 = EDGE_CURVE('',#1987,#1987,#1697,.T.) ;
#2485 = EDGE_CURVE('',#1988,#1988,#1698,.T.) ;
#2486 = EDGE_CURVE('',#1989,#1989,#1699,.T.) ;
#2487 = EDGE_CURVE('',#1986,#1990,#1700,.T.) ;
#2488 = EDGE_CURVE('',#1990,#1990,#1701,.T.) ;
#2489 = EDGE_CURVE('',#1990,#1987,#1162,.T.) ;
#2490 = EDGE_CURVE('',#1988,#1991,#1702,.T.) ;
#2491 = EDGE_CURVE('',#1991,#1991,#1703,.T.) ;
#2492 = EDGE_CURVE('',#1991,#1992,#1163,.T.) ;
#2493 = EDGE_CURVE('',#1992,#1992,#1704,.T.) ;
#2494 = EDGE_CURVE('',#1992,#1989,#1164,.T.) ;
#2495 = EDGE_CURVE('',#1993,#1994,#1165,.T.) ;
#2496 = EDGE_CURVE('',#1993,#1995,#1166,.T.) ;
#2497 = EDGE_CURVE('',#1995,#1996,#1167,.T.) ;
#2498 = EDGE_CURVE('',#1994,#1996,#1168,.T.) ;
#2499 = EDGE_CURVE('',#1997,#1998,#1169,.T.) ;
#2500 = EDGE_CURVE('',#1997,#1993,#1170,.T.) ;
#2501 = EDGE_CURVE('',#1998,#1994,#1171,.T.) ;
#2502 = EDGE_CURVE('',#1995,#1999,#1172,.T.) ;
#2503 = EDGE_CURVE('',#1999,#2000,#1173,.T.) ;
#2504 = EDGE_CURVE('',#1996,#2000,#1174,.T.) ;
#2505 = EDGE_CURVE('',#2000,#2001,#1175,.T.) ;
#2506 = EDGE_CURVE('',#2001,#2002,#1176,.T.) ;
#2507 = EDGE_CURVE('',#2002,#1998,#1177,.T.) ;
#2508 = EDGE_CURVE('',#2003,#2002,#1178,.T.) ;
#2509 = EDGE_CURVE('',#2003,#1997,#1179,.T.) ;
#2510 = EDGE_CURVE('',#1999,#2004,#1180,.T.) ;
#2511 = EDGE_CURVE('',#2004,#2001,#1181,.T.) ;
#2512 = EDGE_CURVE('',#2004,#2003,#1182,.T.) ;
#2513 = EDGE_CURVE('',#2005,#2005,#1705,.T.) ;
#2514 = EDGE_CURVE('',#2006,#2006,#1706,.T.) ;
#2515 = EDGE_CURVE('',#2007,#2007,#1707,.T.) ;
#2516 = EDGE_CURVE('',#2008,#2008,#1708,.T.) ;
#2517 = EDGE_CURVE('',#2005,#2009,#1709,.T.) ;
#2518 = EDGE_CURVE('',#2009,#2009,#1710,.T.) ;
#2519 = EDGE_CURVE('',#2009,#2006,#1183,.T.) ;
#2520 = EDGE_CURVE('',#2007,#2010,#1711,.T.) ;
#2521 = EDGE_CURVE('',#2010,#2010,#1712,.T.) ;
#2522 = EDGE_CURVE('',#2010,#2011,#1184,.T.) ;
#2523 = EDGE_CURVE('',#2011,#2011,#1713,.T.) ;
#2524 = EDGE_CURVE('',#2011,#2008,#1185,.T.) ;
#2525 = EDGE_CURVE('',#2012,#2013,#1186,.T.) ;
#2526 = EDGE_CURVE('',#2012,#2014,#1187,.T.) ;
#2527 = EDGE_CURVE('',#2014,#2015,#1188,.T.) ;
#2528 = EDGE_CURVE('',#2013,#2015,#1189,.T.) ;
#2529 = EDGE_CURVE('',#2016,#2017,#1190,.T.) ;
#2530 = EDGE_CURVE('',#2016,#2012,#1191,.T.) ;
#2531 = EDGE_CURVE('',#2017,#2013,#1192,.T.) ;
#2532 = EDGE_CURVE('',#2014,#2018,#1193,.T.) ;
#2533 = EDGE_CURVE('',#2018,#2019,#1194,.T.) ;
#2534 = EDGE_CURVE('',#2015,#2019,#1195,.T.) ;
#2535 = EDGE_CURVE('',#2019,#2020,#1196,.T.) ;
#2536 = EDGE_CURVE('',#2020,#2021,#1197,.T.) ;
#2537 = EDGE_CURVE('',#2021,#2017,#1198,.T.) ;
#2538 = EDGE_CURVE('',#2022,#2021,#1199,.T.) ;
#2539 = EDGE_CURVE('',#2022,#2016,#1200,.T.) ;
#2540 = EDGE_CURVE('',#2018,#2023,#1201,.T.) ;
#2541 = EDGE_CURVE('',#2023,#2020,#1202,.T.) ;
#2542 = EDGE_CURVE('',#2023,#2022,#1203,.T.) ;
#2543 = EDGE_CURVE('',#2024,#2024,#1714,.T.) ;
#2544 = EDGE_CURVE('',#2025,#2025,#1715,.T.) ;
#2545 = EDGE_CURVE('',#2026,#2026,#1716,.T.) ;
#2546 = EDGE_CURVE('',#2027,#2027,#1717,.T.) ;
#2547 = EDGE_CURVE('',#2024,#2028,#1718,.T.) ;
#2548 = EDGE_CURVE('',#2028,#2028,#1719,.T.) ;
#2549 = EDGE_CURVE('',#2028,#2025,#1204,.T.) ;
#2550 = EDGE_CURVE('',#2026,#2029,#1720,.T.) ;
#2551 = EDGE_CURVE('',#2029,#2029,#1721,.T.) ;
#2552 = EDGE_CURVE('',#2029,#2030,#1205,.T.) ;
#2553 = EDGE_CURVE('',#2030,#2030,#1722,.T.) ;
#2554 = EDGE_CURVE('',#2030,#2027,#1206,.T.) ;
#2555 = ORIENTED_EDGE('',*,*,#2031,.T.) ;
#2556 = ORIENTED_EDGE('',*,*,#2032,.T.) ;
#2557 = ORIENTED_EDGE('',*,*,#2033,.F.) ;
#2558 = ORIENTED_EDGE('',*,*,#2034,.F.) ;
#2559 = ORIENTED_EDGE('',*,*,#2035,.T.) ;
#2560 = ORIENTED_EDGE('',*,*,#2031,.F.) ;
#2561 = ORIENTED_EDGE('',*,*,#2036,.T.) ;
#2562 = ORIENTED_EDGE('',*,*,#2037,.T.) ;
#2563 = ORIENTED_EDGE('',*,*,#2038,.F.) ;
#2564 = ORIENTED_EDGE('',*,*,#2039,.T.) ;
#2565 = ORIENTED_EDGE('',*,*,#2033,.T.) ;
#2566 = ORIENTED_EDGE('',*,*,#2040,.T.) ;
#2567 = ORIENTED_EDGE('',*,*,#2041,.T.) ;
#2568 = ORIENTED_EDGE('',*,*,#2042,.T.) ;
#2569 = ORIENTED_EDGE('',*,*,#2043,.T.) ;
#2570 = ORIENTED_EDGE('',*,*,#2042,.F.) ;
#2571 = ORIENTED_EDGE('',*,*,#2043,.F.) ;
#2572 = ORIENTED_EDGE('',*,*,#2044,.T.) ;
#2573 = ORIENTED_EDGE('',*,*,#2045,.T.) ;
#2574 = ORIENTED_EDGE('',*,*,#2044,.F.) ;
#2575 = ORIENTED_EDGE('',*,*,#2046,.T.) ;
#2576 = ORIENTED_EDGE('',*,*,#2047,.T.) ;
#2577 = ORIENTED_EDGE('',*,*,#2048,.T.) ;
#2578 = ORIENTED_EDGE('',*,*,#2047,.F.) ;
#2579 = ORIENTED_EDGE('',*,*,#2048,.F.) ;
#2580 = ORIENTED_EDGE('',*,*,#2049,.T.) ;
#2581 = ORIENTED_EDGE('',*,*,#2050,.T.) ;
#2582 = ORIENTED_EDGE('',*,*,#2049,.F.) ;
#2583 = ORIENTED_EDGE('',*,*,#2051,.T.) ;
#2584 = ORIENTED_EDGE('',*,*,#2052,.T.) ;
#2585 = ORIENTED_EDGE('',*,*,#2053,.T.) ;
#2586 = ORIENTED_EDGE('',*,*,#2052,.F.) ;
#2587 = ORIENTED_EDGE('',*,*,#2053,.F.) ;
#2588 = ORIENTED_EDGE('',*,*,#2054,.T.) ;
#2589 = ORIENTED_EDGE('',*,*,#2055,.T.) ;
#2590 = ORIENTED_EDGE('',*,*,#2054,.F.) ;
#2591 = ORIENTED_EDGE('',*,*,#2056,.T.) ;
#2592 = ORIENTED_EDGE('',*,*,#2057,.T.) ;
#2593 = ORIENTED_EDGE('',*,*,#2058,.T.) ;
#2594 = ORIENTED_EDGE('',*,*,#2057,.F.) ;
#2595 = ORIENTED_EDGE('',*,*,#2058,.F.) ;
#2596 = ORIENTED_EDGE('',*,*,#2059,.T.) ;
#2597 = ORIENTED_EDGE('',*,*,#2060,.T.) ;
#2598 = ORIENTED_EDGE('',*,*,#2059,.F.) ;
#2599 = ORIENTED_EDGE('',*,*,#2061,.T.) ;
#2600 = ORIENTED_EDGE('',*,*,#2038,.T.) ;
#2601 = ORIENTED_EDGE('',*,*,#2062,.T.) ;
#2602 = ORIENTED_EDGE('',*,*,#2063,.T.) ;
#2603 = ORIENTED_EDGE('',*,*,#2064,.T.) ;
#2604 = ORIENTED_EDGE('',*,*,#2065,.T.) ;
#2605 = ORIENTED_EDGE('',*,*,#2066,.T.) ;
#2606 = ORIENTED_EDGE('',*,*,#2067,.T.) ;
#2607 = ORIENTED_EDGE('',*,*,#2068,.T.) ;
#2608 = ORIENTED_EDGE('',*,*,#2069,.T.) ;
#2609 = ORIENTED_EDGE('',*,*,#2070,.T.) ;
#2610 = ORIENTED_EDGE('',*,*,#2071,.T.) ;
#2611 = ORIENTED_EDGE('',*,*,#2072,.T.) ;
#2612 = ORIENTED_EDGE('',*,*,#2073,.T.) ;
#2613 = ORIENTED_EDGE('',*,*,#2074,.T.) ;
#2614 = ORIENTED_EDGE('',*,*,#2075,.T.) ;
#2615 = ORIENTED_EDGE('',*,*,#2076,.T.) ;
#2616 = ORIENTED_EDGE('',*,*,#2077,.T.) ;
#2617 = ORIENTED_EDGE('',*,*,#2078,.T.) ;
#2618 = ORIENTED_EDGE('',*,*,#2079,.T.) ;
#2619 = ORIENTED_EDGE('',*,*,#2080,.T.) ;
#2620 = ORIENTED_EDGE('',*,*,#2081,.T.) ;
#2621 = ORIENTED_EDGE('',*,*,#2082,.T.) ;
#2622 = ORIENTED_EDGE('',*,*,#2083,.T.) ;
#2623 = ORIENTED_EDGE('',*,*,#2084,.T.) ;
#2624 = ORIENTED_EDGE('',*,*,#2085,.T.) ;
#2625 = ORIENTED_EDGE('',*,*,#2086,.T.) ;
#2626 = ORIENTED_EDGE('',*,*,#2087,.T.) ;
#2627 = ORIENTED_EDGE('',*,*,#2088,.F.) ;
#2628 = ORIENTED_EDGE('',*,*,#2064,.F.) ;
#2629 = ORIENTED_EDGE('',*,*,#2088,.T.) ;
#2630 = ORIENTED_EDGE('',*,*,#2089,.T.) ;
#2631 = ORIENTED_EDGE('',*,*,#2090,.F.) ;
#2632 = ORIENTED_EDGE('',*,*,#2065,.F.) ;
#2633 = ORIENTED_EDGE('',*,*,#2090,.T.) ;
#2634 = ORIENTED_EDGE('',*,*,#2091,.T.) ;
#2635 = ORIENTED_EDGE('',*,*,#2092,.F.) ;
#2636 = ORIENTED_EDGE('',*,*,#2092,.T.) ;
#2637 = ORIENTED_EDGE('',*,*,#2093,.T.) ;
#2638 = ORIENTED_EDGE('',*,*,#2094,.F.) ;
#2639 = ORIENTED_EDGE('',*,*,#2066,.F.) ;
#2640 = ORIENTED_EDGE('',*,*,#2094,.T.) ;
#2641 = ORIENTED_EDGE('',*,*,#2095,.T.) ;
#2642 = ORIENTED_EDGE('',*,*,#2096,.F.) ;
#2643 = ORIENTED_EDGE('',*,*,#2096,.T.) ;
#2644 = ORIENTED_EDGE('',*,*,#2097,.T.) ;
#2645 = ORIENTED_EDGE('',*,*,#2098,.F.) ;
#2646 = ORIENTED_EDGE('',*,*,#2067,.F.) ;
#2647 = ORIENTED_EDGE('',*,*,#2098,.T.) ;
#2648 = ORIENTED_EDGE('',*,*,#2099,.T.) ;
#2649 = ORIENTED_EDGE('',*,*,#2100,.F.) ;
#2650 = ORIENTED_EDGE('',*,*,#2100,.T.) ;
#2651 = ORIENTED_EDGE('',*,*,#2101,.T.) ;
#2652 = ORIENTED_EDGE('',*,*,#2102,.F.) ;
#2653 = ORIENTED_EDGE('',*,*,#2068,.F.) ;
#2654 = ORIENTED_EDGE('',*,*,#2102,.T.) ;
#2655 = ORIENTED_EDGE('',*,*,#2103,.T.) ;
#2656 = ORIENTED_EDGE('',*,*,#2104,.F.) ;
#2657 = ORIENTED_EDGE('',*,*,#2104,.T.) ;
#2658 = ORIENTED_EDGE('',*,*,#2105,.T.) ;
#2659 = ORIENTED_EDGE('',*,*,#2106,.F.) ;
#2660 = ORIENTED_EDGE('',*,*,#2069,.F.) ;
#2661 = ORIENTED_EDGE('',*,*,#2106,.T.) ;
#2662 = ORIENTED_EDGE('',*,*,#2107,.T.) ;
#2663 = ORIENTED_EDGE('',*,*,#2108,.F.) ;
#2664 = ORIENTED_EDGE('',*,*,#2070,.F.) ;
#2665 = ORIENTED_EDGE('',*,*,#2108,.T.) ;
#2666 = ORIENTED_EDGE('',*,*,#2109,.T.) ;
#2667 = ORIENTED_EDGE('',*,*,#2110,.F.) ;
#2668 = ORIENTED_EDGE('',*,*,#2071,.F.) ;
#2669 = ORIENTED_EDGE('',*,*,#2110,.T.) ;
#2670 = ORIENTED_EDGE('',*,*,#2111,.T.) ;
#2671 = ORIENTED_EDGE('',*,*,#2112,.F.) ;
#2672 = ORIENTED_EDGE('',*,*,#2072,.F.) ;
#2673 = ORIENTED_EDGE('',*,*,#2112,.T.) ;
#2674 = ORIENTED_EDGE('',*,*,#2113,.T.) ;
#2675 = ORIENTED_EDGE('',*,*,#2114,.F.) ;
#2676 = ORIENTED_EDGE('',*,*,#2073,.F.) ;
#2677 = ORIENTED_EDGE('',*,*,#2114,.T.) ;
#2678 = ORIENTED_EDGE('',*,*,#2115,.T.) ;
#2679 = ORIENTED_EDGE('',*,*,#2116,.F.) ;
#2680 = ORIENTED_EDGE('',*,*,#2116,.T.) ;
#2681 = ORIENTED_EDGE('',*,*,#2117,.T.) ;
#2682 = ORIENTED_EDGE('',*,*,#2118,.F.) ;
#2683 = ORIENTED_EDGE('',*,*,#2074,.F.) ;
#2684 = ORIENTED_EDGE('',*,*,#2118,.T.) ;
#2685 = ORIENTED_EDGE('',*,*,#2119,.T.) ;
#2686 = ORIENTED_EDGE('',*,*,#2120,.F.) ;
#2687 = ORIENTED_EDGE('',*,*,#2120,.T.) ;
#2688 = ORIENTED_EDGE('',*,*,#2121,.T.) ;
#2689 = ORIENTED_EDGE('',*,*,#2122,.F.) ;
#2690 = ORIENTED_EDGE('',*,*,#2075,.F.) ;
#2691 = ORIENTED_EDGE('',*,*,#2122,.T.) ;
#2692 = ORIENTED_EDGE('',*,*,#2123,.T.) ;
#2693 = ORIENTED_EDGE('',*,*,#2124,.F.) ;
#2694 = ORIENTED_EDGE('',*,*,#2076,.F.) ;
#2695 = ORIENTED_EDGE('',*,*,#2124,.T.) ;
#2696 = ORIENTED_EDGE('',*,*,#2125,.T.) ;
#2697 = ORIENTED_EDGE('',*,*,#2126,.F.) ;
#2698 = ORIENTED_EDGE('',*,*,#2077,.F.) ;
#2699 = ORIENTED_EDGE('',*,*,#2126,.T.) ;
#2700 = ORIENTED_EDGE('',*,*,#2127,.T.) ;
#2701 = ORIENTED_EDGE('',*,*,#2128,.F.) ;
#2702 = ORIENTED_EDGE('',*,*,#2078,.F.) ;
#2703 = ORIENTED_EDGE('',*,*,#2128,.T.) ;
#2704 = ORIENTED_EDGE('',*,*,#2129,.T.) ;
#2705 = ORIENTED_EDGE('',*,*,#2130,.F.) ;
#2706 = ORIENTED_EDGE('',*,*,#2079,.F.) ;
#2707 = ORIENTED_EDGE('',*,*,#2130,.T.) ;
#2708 = ORIENTED_EDGE('',*,*,#2131,.T.) ;
#2709 = ORIENTED_EDGE('',*,*,#2132,.F.) ;
#2710 = ORIENTED_EDGE('',*,*,#2132,.T.) ;
#2711 = ORIENTED_EDGE('',*,*,#2133,.T.) ;
#2712 = ORIENTED_EDGE('',*,*,#2134,.F.) ;
#2713 = ORIENTED_EDGE('',*,*,#2080,.F.) ;
#2714 = ORIENTED_EDGE('',*,*,#2134,.T.) ;
#2715 = ORIENTED_EDGE('',*,*,#2135,.T.) ;
#2716 = ORIENTED_EDGE('',*,*,#2136,.F.) ;
#2717 = ORIENTED_EDGE('',*,*,#2136,.T.) ;
#2718 = ORIENTED_EDGE('',*,*,#2137,.T.) ;
#2719 = ORIENTED_EDGE('',*,*,#2138,.F.) ;
#2720 = ORIENTED_EDGE('',*,*,#2081,.F.) ;
#2721 = ORIENTED_EDGE('',*,*,#2138,.T.) ;
#2722 = ORIENTED_EDGE('',*,*,#2139,.T.) ;
#2723 = ORIENTED_EDGE('',*,*,#2140,.F.) ;
#2724 = ORIENTED_EDGE('',*,*,#2140,.T.) ;
#2725 = ORIENTED_EDGE('',*,*,#2141,.T.) ;
#2726 = ORIENTED_EDGE('',*,*,#2142,.F.) ;
#2727 = ORIENTED_EDGE('',*,*,#2082,.F.) ;
#2728 = ORIENTED_EDGE('',*,*,#2142,.T.) ;
#2729 = ORIENTED_EDGE('',*,*,#2143,.T.) ;
#2730 = ORIENTED_EDGE('',*,*,#2144,.F.) ;
#2731 = ORIENTED_EDGE('',*,*,#2144,.T.) ;
#2732 = ORIENTED_EDGE('',*,*,#2145,.T.) ;
#2733 = ORIENTED_EDGE('',*,*,#2146,.F.) ;
#2734 = ORIENTED_EDGE('',*,*,#2083,.F.) ;
#2735 = ORIENTED_EDGE('',*,*,#2146,.T.) ;
#2736 = ORIENTED_EDGE('',*,*,#2147,.T.) ;
#2737 = ORIENTED_EDGE('',*,*,#2148,.F.) ;
#2738 = ORIENTED_EDGE('',*,*,#2084,.F.) ;
#2739 = ORIENTED_EDGE('',*,*,#2149,.T.) ;
#2740 = ORIENTED_EDGE('',*,*,#2085,.F.) ;
#2741 = ORIENTED_EDGE('',*,*,#2148,.T.) ;
#2742 = ORIENTED_EDGE('',*,*,#2150,.T.) ;
#2743 = ORIENTED_EDGE('',*,*,#2151,.T.) ;
#2744 = ORIENTED_EDGE('',*,*,#2086,.F.) ;
#2745 = ORIENTED_EDGE('',*,*,#2063,.F.) ;
#2746 = ORIENTED_EDGE('',*,*,#2152,.T.) ;
#2747 = ORIENTED_EDGE('',*,*,#2153,.F.) ;
#2748 = ORIENTED_EDGE('',*,*,#2154,.F.) ;
#2749 = ORIENTED_EDGE('',*,*,#2155,.F.) ;
#2750 = ORIENTED_EDGE('',*,*,#2156,.F.) ;
#2751 = ORIENTED_EDGE('',*,*,#2157,.F.) ;
#2752 = ORIENTED_EDGE('',*,*,#2158,.F.) ;
#2753 = ORIENTED_EDGE('',*,*,#2159,.F.) ;
#2754 = ORIENTED_EDGE('',*,*,#2160,.F.) ;
#2755 = ORIENTED_EDGE('',*,*,#2161,.F.) ;
#2756 = ORIENTED_EDGE('',*,*,#2162,.F.) ;
#2757 = ORIENTED_EDGE('',*,*,#2163,.F.) ;
#2758 = ORIENTED_EDGE('',*,*,#2164,.F.) ;
#2759 = ORIENTED_EDGE('',*,*,#2165,.F.) ;
#2760 = ORIENTED_EDGE('',*,*,#2166,.F.) ;
#2761 = ORIENTED_EDGE('',*,*,#2167,.F.) ;
#2762 = ORIENTED_EDGE('',*,*,#2168,.F.) ;
#2763 = ORIENTED_EDGE('',*,*,#2169,.F.) ;
#2764 = ORIENTED_EDGE('',*,*,#2170,.F.) ;
#2765 = ORIENTED_EDGE('',*,*,#2171,.F.) ;
#2766 = ORIENTED_EDGE('',*,*,#2172,.F.) ;
#2767 = ORIENTED_EDGE('',*,*,#2173,.F.) ;
#2768 = ORIENTED_EDGE('',*,*,#2174,.F.) ;
#2769 = ORIENTED_EDGE('',*,*,#2175,.F.) ;
#2770 = ORIENTED_EDGE('',*,*,#2176,.F.) ;
#2771 = ORIENTED_EDGE('',*,*,#2037,.F.) ;
#2772 = ORIENTED_EDGE('',*,*,#2177,.F.) ;
#2773 = ORIENTED_EDGE('',*,*,#2178,.T.) ;
#2774 = ORIENTED_EDGE('',*,*,#2179,.F.) ;
#2775 = ORIENTED_EDGE('',*,*,#2107,.F.) ;
#2776 = ORIENTED_EDGE('',*,*,#2180,.T.) ;
#2777 = ORIENTED_EDGE('',*,*,#2181,.T.) ;
#2778 = ORIENTED_EDGE('',*,*,#2182,.F.) ;
#2779 = ORIENTED_EDGE('',*,*,#2111,.F.) ;
#2780 = ORIENTED_EDGE('',*,*,#2183,.T.) ;
#2781 = ORIENTED_EDGE('',*,*,#2184,.T.) ;
#2782 = ORIENTED_EDGE('',*,*,#2185,.F.) ;
#2783 = ORIENTED_EDGE('',*,*,#2123,.F.) ;
#2784 = ORIENTED_EDGE('',*,*,#2186,.T.) ;
#2785 = ORIENTED_EDGE('',*,*,#2187,.T.) ;
#2786 = ORIENTED_EDGE('',*,*,#2188,.F.) ;
#2787 = ORIENTED_EDGE('',*,*,#2127,.F.) ;
#2788 = ORIENTED_EDGE('',*,*,#2189,.T.) ;
#2789 = ORIENTED_EDGE('',*,*,#2190,.T.) ;
#2790 = ORIENTED_EDGE('',*,*,#2191,.F.) ;
#2791 = ORIENTED_EDGE('',*,*,#2147,.F.) ;
#2792 = ORIENTED_EDGE('',*,*,#2192,.T.) ;
#2793 = ORIENTED_EDGE('',*,*,#2193,.T.) ;
#2794 = ORIENTED_EDGE('',*,*,#2194,.F.) ;
#2795 = ORIENTED_EDGE('',*,*,#2087,.F.) ;
#2796 = ORIENTED_EDGE('',*,*,#2195,.T.) ;
#2797 = ORIENTED_EDGE('',*,*,#2196,.T.) ;
#2798 = ORIENTED_EDGE('',*,*,#2195,.F.) ;
#2799 = ORIENTED_EDGE('',*,*,#2151,.F.) ;
#2800 = ORIENTED_EDGE('',*,*,#2197,.F.) ;
#2801 = ORIENTED_EDGE('',*,*,#2189,.F.) ;
#2802 = ORIENTED_EDGE('',*,*,#2125,.F.) ;
#2803 = ORIENTED_EDGE('',*,*,#2185,.T.) ;
#2804 = ORIENTED_EDGE('',*,*,#2198,.T.) ;
#2805 = ORIENTED_EDGE('',*,*,#2183,.F.) ;
#2806 = ORIENTED_EDGE('',*,*,#2109,.F.) ;
#2807 = ORIENTED_EDGE('',*,*,#2179,.T.) ;
#2808 = ORIENTED_EDGE('',*,*,#2199,.T.) ;
#2809 = ORIENTED_EDGE('',*,*,#2200,.T.) ;
#2810 = ORIENTED_EDGE('',*,*,#2150,.F.) ;
#2811 = ORIENTED_EDGE('',*,*,#2191,.T.) ;
#2812 = ORIENTED_EDGE('',*,*,#2201,.T.) ;
#2813 = ORIENTED_EDGE('',*,*,#2197,.T.) ;
#2814 = ORIENTED_EDGE('',*,*,#2152,.F.) ;
#2815 = ORIENTED_EDGE('',*,*,#2062,.F.) ;
#2816 = ORIENTED_EDGE('',*,*,#2040,.F.) ;
#2817 = ORIENTED_EDGE('',*,*,#2032,.F.) ;
#2818 = ORIENTED_EDGE('',*,*,#2035,.F.) ;
#2819 = ORIENTED_EDGE('',*,*,#2176,.T.) ;
#2820 = ORIENTED_EDGE('',*,*,#2202,.F.) ;
#2821 = ORIENTED_EDGE('',*,*,#2041,.F.) ;
#2822 = ORIENTED_EDGE('',*,*,#2046,.F.) ;
#2823 = ORIENTED_EDGE('',*,*,#2177,.T.) ;
#2824 = ORIENTED_EDGE('',*,*,#2036,.F.) ;
#2825 = ORIENTED_EDGE('',*,*,#2034,.T.) ;
#2826 = ORIENTED_EDGE('',*,*,#2039,.F.) ;
#2827 = ORIENTED_EDGE('',*,*,#2061,.F.) ;
#2828 = ORIENTED_EDGE('',*,*,#2149,.F.) ;
#2829 = ORIENTED_EDGE('',*,*,#2200,.F.) ;
#2830 = ORIENTED_EDGE('',*,*,#2203,.F.) ;
#2831 = ORIENTED_EDGE('',*,*,#2056,.F.) ;
#2832 = ORIENTED_EDGE('',*,*,#2051,.F.) ;
#2833 = ORIENTED_EDGE('',*,*,#2204,.T.) ;
#2834 = ORIENTED_EDGE('',*,*,#2095,.F.) ;
#2835 = ORIENTED_EDGE('',*,*,#2205,.F.) ;
#2836 = ORIENTED_EDGE('',*,*,#2206,.T.) ;
#2837 = ORIENTED_EDGE('',*,*,#2207,.T.) ;
#2838 = ORIENTED_EDGE('',*,*,#2097,.F.) ;
#2839 = ORIENTED_EDGE('',*,*,#2204,.F.) ;
#2840 = ORIENTED_EDGE('',*,*,#2208,.T.) ;
#2841 = ORIENTED_EDGE('',*,*,#2209,.T.) ;
#2842 = ORIENTED_EDGE('',*,*,#2099,.F.) ;
#2843 = ORIENTED_EDGE('',*,*,#2207,.F.) ;
#2844 = ORIENTED_EDGE('',*,*,#2210,.T.) ;
#2845 = ORIENTED_EDGE('',*,*,#2180,.F.) ;
#2846 = ORIENTED_EDGE('',*,*,#2105,.F.) ;
#2847 = ORIENTED_EDGE('',*,*,#2211,.F.) ;
#2848 = ORIENTED_EDGE('',*,*,#2212,.T.) ;
#2849 = ORIENTED_EDGE('',*,*,#2213,.T.) ;
#2850 = ORIENTED_EDGE('',*,*,#2101,.F.) ;
#2851 = ORIENTED_EDGE('',*,*,#2209,.F.) ;
#2852 = ORIENTED_EDGE('',*,*,#2214,.T.) ;
#2853 = ORIENTED_EDGE('',*,*,#2050,.F.) ;
#2854 = ORIENTED_EDGE('',*,*,#2045,.F.) ;
#2855 = ORIENTED_EDGE('',*,*,#2211,.T.) ;
#2856 = ORIENTED_EDGE('',*,*,#2103,.F.) ;
#2857 = ORIENTED_EDGE('',*,*,#2213,.F.) ;
#2858 = ORIENTED_EDGE('',*,*,#2215,.T.) ;
#2859 = ORIENTED_EDGE('',*,*,#2216,.T.) ;
#2860 = ORIENTED_EDGE('',*,*,#2113,.F.) ;
#2861 = ORIENTED_EDGE('',*,*,#2182,.T.) ;
#2862 = ORIENTED_EDGE('',*,*,#2217,.T.) ;
#2863 = ORIENTED_EDGE('',*,*,#2218,.T.) ;
#2864 = ORIENTED_EDGE('',*,*,#2115,.F.) ;
#2865 = ORIENTED_EDGE('',*,*,#2216,.F.) ;
#2866 = ORIENTED_EDGE('',*,*,#2219,.T.) ;
#2867 = ORIENTED_EDGE('',*,*,#2220,.T.) ;
#2868 = ORIENTED_EDGE('',*,*,#2186,.F.) ;
#2869 = ORIENTED_EDGE('',*,*,#2121,.F.) ;
#2870 = ORIENTED_EDGE('',*,*,#2221,.F.) ;
#2871 = ORIENTED_EDGE('',*,*,#2222,.T.) ;
#2872 = ORIENTED_EDGE('',*,*,#2117,.F.) ;
#2873 = ORIENTED_EDGE('',*,*,#2218,.F.) ;
#2874 = ORIENTED_EDGE('',*,*,#2223,.T.) ;
#2875 = ORIENTED_EDGE('',*,*,#2221,.T.) ;
#2876 = ORIENTED_EDGE('',*,*,#2119,.F.) ;
#2877 = ORIENTED_EDGE('',*,*,#2222,.F.) ;
#2878 = ORIENTED_EDGE('',*,*,#2224,.T.) ;
#2879 = ORIENTED_EDGE('',*,*,#2225,.T.) ;
#2880 = ORIENTED_EDGE('',*,*,#2226,.T.) ;
#2881 = ORIENTED_EDGE('',*,*,#2129,.F.) ;
#2882 = ORIENTED_EDGE('',*,*,#2188,.T.) ;
#2883 = ORIENTED_EDGE('',*,*,#2227,.T.) ;
#2884 = ORIENTED_EDGE('',*,*,#2131,.F.) ;
#2885 = ORIENTED_EDGE('',*,*,#2226,.F.) ;
#2886 = ORIENTED_EDGE('',*,*,#2228,.T.) ;
#2887 = ORIENTED_EDGE('',*,*,#2229,.T.) ;
#2888 = ORIENTED_EDGE('',*,*,#2133,.F.) ;
#2889 = ORIENTED_EDGE('',*,*,#2227,.F.) ;
#2890 = ORIENTED_EDGE('',*,*,#2230,.T.) ;
#2891 = ORIENTED_EDGE('',*,*,#2060,.F.) ;
#2892 = ORIENTED_EDGE('',*,*,#2055,.F.) ;
#2893 = ORIENTED_EDGE('',*,*,#2231,.T.) ;
#2894 = ORIENTED_EDGE('',*,*,#2135,.F.) ;
#2895 = ORIENTED_EDGE('',*,*,#2229,.F.) ;
#2896 = ORIENTED_EDGE('',*,*,#2232,.T.) ;
#2897 = ORIENTED_EDGE('',*,*,#2233,.T.) ;
#2898 = ORIENTED_EDGE('',*,*,#2234,.T.) ;
#2899 = ORIENTED_EDGE('',*,*,#2137,.F.) ;
#2900 = ORIENTED_EDGE('',*,*,#2231,.F.) ;
#2901 = ORIENTED_EDGE('',*,*,#2235,.T.) ;
#2902 = ORIENTED_EDGE('',*,*,#2139,.F.) ;
#2903 = ORIENTED_EDGE('',*,*,#2234,.F.) ;
#2904 = ORIENTED_EDGE('',*,*,#2236,.T.) ;
#2905 = ORIENTED_EDGE('',*,*,#2237,.T.) ;
#2906 = ORIENTED_EDGE('',*,*,#2238,.T.) ;
#2907 = ORIENTED_EDGE('',*,*,#2089,.F.) ;
#2908 = ORIENTED_EDGE('',*,*,#2194,.T.) ;
#2909 = ORIENTED_EDGE('',*,*,#2239,.T.) ;
#2910 = ORIENTED_EDGE('',*,*,#2205,.T.) ;
#2911 = ORIENTED_EDGE('',*,*,#2093,.F.) ;
#2912 = ORIENTED_EDGE('',*,*,#2240,.F.) ;
#2913 = ORIENTED_EDGE('',*,*,#2240,.T.) ;
#2914 = ORIENTED_EDGE('',*,*,#2091,.F.) ;
#2915 = ORIENTED_EDGE('',*,*,#2238,.F.) ;
#2916 = ORIENTED_EDGE('',*,*,#2241,.T.) ;
#2917 = ORIENTED_EDGE('',*,*,#2192,.F.) ;
#2918 = ORIENTED_EDGE('',*,*,#2145,.F.) ;
#2919 = ORIENTED_EDGE('',*,*,#2242,.F.) ;
#2920 = ORIENTED_EDGE('',*,*,#2243,.T.) ;
#2921 = ORIENTED_EDGE('',*,*,#2244,.T.) ;
#2922 = ORIENTED_EDGE('',*,*,#2141,.F.) ;
#2923 = ORIENTED_EDGE('',*,*,#2235,.F.) ;
#2924 = ORIENTED_EDGE('',*,*,#2245,.T.) ;
#2925 = ORIENTED_EDGE('',*,*,#2242,.T.) ;
#2926 = ORIENTED_EDGE('',*,*,#2143,.F.) ;
#2927 = ORIENTED_EDGE('',*,*,#2244,.F.) ;
#2928 = ORIENTED_EDGE('',*,*,#2246,.T.) ;
#2929 = ORIENTED_EDGE('',*,*,#2247,.T.) ;
#2930 = ORIENTED_EDGE('',*,*,#2174,.T.) ;
#2931 = ORIENTED_EDGE('',*,*,#2248,.F.) ;
#2932 = ORIENTED_EDGE('',*,*,#2193,.F.) ;
#2933 = ORIENTED_EDGE('',*,*,#2248,.T.) ;
#2934 = ORIENTED_EDGE('',*,*,#2173,.T.) ;
#2935 = ORIENTED_EDGE('',*,*,#2249,.F.) ;
#2936 = ORIENTED_EDGE('',*,*,#2237,.F.) ;
#2937 = ORIENTED_EDGE('',*,*,#2249,.T.) ;
#2938 = ORIENTED_EDGE('',*,*,#2250,.F.) ;
#2939 = ORIENTED_EDGE('',*,*,#2241,.F.) ;
#2940 = ORIENTED_EDGE('',*,*,#2250,.T.) ;
#2941 = ORIENTED_EDGE('',*,*,#2172,.T.) ;
#2942 = ORIENTED_EDGE('',*,*,#2251,.F.) ;
#2943 = ORIENTED_EDGE('',*,*,#2239,.F.) ;
#2944 = ORIENTED_EDGE('',*,*,#2251,.T.) ;
#2945 = ORIENTED_EDGE('',*,*,#2252,.F.) ;
#2946 = ORIENTED_EDGE('',*,*,#2206,.F.) ;
#2947 = ORIENTED_EDGE('',*,*,#2252,.T.) ;
#2948 = ORIENTED_EDGE('',*,*,#2171,.T.) ;
#2949 = ORIENTED_EDGE('',*,*,#2253,.F.) ;
#2950 = ORIENTED_EDGE('',*,*,#2208,.F.) ;
#2951 = ORIENTED_EDGE('',*,*,#2253,.T.) ;
#2952 = ORIENTED_EDGE('',*,*,#2254,.F.) ;
#2953 = ORIENTED_EDGE('',*,*,#2210,.F.) ;
#2954 = ORIENTED_EDGE('',*,*,#2254,.T.) ;
#2955 = ORIENTED_EDGE('',*,*,#2170,.T.) ;
#2956 = ORIENTED_EDGE('',*,*,#2255,.F.) ;
#2957 = ORIENTED_EDGE('',*,*,#2214,.F.) ;
#2958 = ORIENTED_EDGE('',*,*,#2255,.T.) ;
#2959 = ORIENTED_EDGE('',*,*,#2256,.F.) ;
#2960 = ORIENTED_EDGE('',*,*,#2215,.F.) ;
#2961 = ORIENTED_EDGE('',*,*,#2256,.T.) ;
#2962 = ORIENTED_EDGE('',*,*,#2169,.T.) ;
#2963 = ORIENTED_EDGE('',*,*,#2257,.F.) ;
#2964 = ORIENTED_EDGE('',*,*,#2212,.F.) ;
#2965 = ORIENTED_EDGE('',*,*,#2257,.T.) ;
#2966 = ORIENTED_EDGE('',*,*,#2168,.T.) ;
#2967 = ORIENTED_EDGE('',*,*,#2258,.F.) ;
#2968 = ORIENTED_EDGE('',*,*,#2178,.F.) ;
#2969 = ORIENTED_EDGE('',*,*,#2258,.T.) ;
#2970 = ORIENTED_EDGE('',*,*,#2167,.T.) ;
#2971 = ORIENTED_EDGE('',*,*,#2259,.F.) ;
#2972 = ORIENTED_EDGE('',*,*,#2199,.F.) ;
#2973 = ORIENTED_EDGE('',*,*,#2259,.T.) ;
#2974 = ORIENTED_EDGE('',*,*,#2166,.T.) ;
#2975 = ORIENTED_EDGE('',*,*,#2260,.F.) ;
#2976 = ORIENTED_EDGE('',*,*,#2181,.F.) ;
#2977 = ORIENTED_EDGE('',*,*,#2260,.T.) ;
#2978 = ORIENTED_EDGE('',*,*,#2165,.T.) ;
#2979 = ORIENTED_EDGE('',*,*,#2261,.F.) ;
#2980 = ORIENTED_EDGE('',*,*,#2217,.F.) ;
#2981 = ORIENTED_EDGE('',*,*,#2261,.T.) ;
#2982 = ORIENTED_EDGE('',*,*,#2262,.F.) ;
#2983 = ORIENTED_EDGE('',*,*,#2219,.F.) ;
#2984 = ORIENTED_EDGE('',*,*,#2262,.T.) ;
#2985 = ORIENTED_EDGE('',*,*,#2164,.T.) ;
#2986 = ORIENTED_EDGE('',*,*,#2263,.F.) ;
#2987 = ORIENTED_EDGE('',*,*,#2223,.F.) ;
#2988 = ORIENTED_EDGE('',*,*,#2263,.T.) ;
#2989 = ORIENTED_EDGE('',*,*,#2264,.F.) ;
#2990 = ORIENTED_EDGE('',*,*,#2224,.F.) ;
#2991 = ORIENTED_EDGE('',*,*,#2264,.T.) ;
#2992 = ORIENTED_EDGE('',*,*,#2163,.T.) ;
#2993 = ORIENTED_EDGE('',*,*,#2265,.F.) ;
#2994 = ORIENTED_EDGE('',*,*,#2220,.F.) ;
#2995 = ORIENTED_EDGE('',*,*,#2265,.T.) ;
#2996 = ORIENTED_EDGE('',*,*,#2162,.T.) ;
#2997 = ORIENTED_EDGE('',*,*,#2266,.F.) ;
#2998 = ORIENTED_EDGE('',*,*,#2184,.F.) ;
#2999 = ORIENTED_EDGE('',*,*,#2266,.T.) ;
#3000 = ORIENTED_EDGE('',*,*,#2161,.T.) ;
#3001 = ORIENTED_EDGE('',*,*,#2267,.F.) ;
#3002 = ORIENTED_EDGE('',*,*,#2198,.F.) ;
#3003 = ORIENTED_EDGE('',*,*,#2267,.T.) ;
#3004 = ORIENTED_EDGE('',*,*,#2160,.T.) ;
#3005 = ORIENTED_EDGE('',*,*,#2268,.F.) ;
#3006 = ORIENTED_EDGE('',*,*,#2187,.F.) ;
#3007 = ORIENTED_EDGE('',*,*,#2268,.T.) ;
#3008 = ORIENTED_EDGE('',*,*,#2159,.T.) ;
#3009 = ORIENTED_EDGE('',*,*,#2269,.F.) ;
#3010 = ORIENTED_EDGE('',*,*,#2225,.F.) ;
#3011 = ORIENTED_EDGE('',*,*,#2269,.T.) ;
#3012 = ORIENTED_EDGE('',*,*,#2270,.F.) ;
#3013 = ORIENTED_EDGE('',*,*,#2228,.F.) ;
#3014 = ORIENTED_EDGE('',*,*,#2270,.T.) ;
#3015 = ORIENTED_EDGE('',*,*,#2158,.T.) ;
#3016 = ORIENTED_EDGE('',*,*,#2271,.F.) ;
#3017 = ORIENTED_EDGE('',*,*,#2230,.F.) ;
#3018 = ORIENTED_EDGE('',*,*,#2271,.T.) ;
#3019 = ORIENTED_EDGE('',*,*,#2272,.F.) ;
#3020 = ORIENTED_EDGE('',*,*,#2232,.F.) ;
#3021 = ORIENTED_EDGE('',*,*,#2272,.T.) ;
#3022 = ORIENTED_EDGE('',*,*,#2157,.T.) ;
#3023 = ORIENTED_EDGE('',*,*,#2273,.F.) ;
#3024 = ORIENTED_EDGE('',*,*,#2233,.F.) ;
#3025 = ORIENTED_EDGE('',*,*,#2273,.T.) ;
#3026 = ORIENTED_EDGE('',*,*,#2274,.F.) ;
#3027 = ORIENTED_EDGE('',*,*,#2236,.F.) ;
#3028 = ORIENTED_EDGE('',*,*,#2274,.T.) ;
#3029 = ORIENTED_EDGE('',*,*,#2156,.T.) ;
#3030 = ORIENTED_EDGE('',*,*,#2275,.F.) ;
#3031 = ORIENTED_EDGE('',*,*,#2245,.F.) ;
#3032 = ORIENTED_EDGE('',*,*,#2275,.T.) ;
#3033 = ORIENTED_EDGE('',*,*,#2276,.F.) ;
#3034 = ORIENTED_EDGE('',*,*,#2246,.F.) ;
#3035 = ORIENTED_EDGE('',*,*,#2276,.T.) ;
#3036 = ORIENTED_EDGE('',*,*,#2155,.T.) ;
#3037 = ORIENTED_EDGE('',*,*,#2277,.F.) ;
#3038 = ORIENTED_EDGE('',*,*,#2243,.F.) ;
#3039 = ORIENTED_EDGE('',*,*,#2277,.T.) ;
#3040 = ORIENTED_EDGE('',*,*,#2154,.T.) ;
#3041 = ORIENTED_EDGE('',*,*,#2278,.F.) ;
#3042 = ORIENTED_EDGE('',*,*,#2190,.F.) ;
#3043 = ORIENTED_EDGE('',*,*,#2201,.F.) ;
#3044 = ORIENTED_EDGE('',*,*,#2278,.T.) ;
#3045 = ORIENTED_EDGE('',*,*,#2153,.T.) ;
#3046 = ORIENTED_EDGE('',*,*,#2203,.T.) ;
#3047 = ORIENTED_EDGE('',*,*,#2202,.T.) ;
#3048 = ORIENTED_EDGE('',*,*,#2175,.T.) ;
#3049 = ORIENTED_EDGE('',*,*,#2247,.F.) ;
#3050 = ORIENTED_EDGE('',*,*,#2196,.F.) ;
#3051 = ORIENTED_EDGE('',*,*,#2279,.T.) ;
#3052 = ORIENTED_EDGE('',*,*,#2280,.F.) ;
#3053 = ORIENTED_EDGE('',*,*,#2281,.T.) ;
#3054 = ORIENTED_EDGE('',*,*,#2282,.T.) ;
#3055 = ORIENTED_EDGE('',*,*,#2280,.T.) ;
#3056 = ORIENTED_EDGE('',*,*,#2283,.T.) ;
#3057 = ORIENTED_EDGE('',*,*,#2284,.F.) ;
#3058 = ORIENTED_EDGE('',*,*,#2285,.F.) ;
#3059 = ORIENTED_EDGE('',*,*,#2286,.F.) ;
#3060 = ORIENTED_EDGE('',*,*,#2287,.T.) ;
#3061 = ORIENTED_EDGE('',*,*,#2284,.T.) ;
#3062 = ORIENTED_EDGE('',*,*,#2288,.T.) ;
#3063 = ORIENTED_EDGE('',*,*,#2289,.T.) ;
#3064 = ORIENTED_EDGE('',*,*,#2286,.T.) ;
#3065 = ORIENTED_EDGE('',*,*,#2290,.T.) ;
#3066 = ORIENTED_EDGE('',*,*,#2291,.T.) ;
#3067 = ORIENTED_EDGE('',*,*,#2292,.T.) ;
#3068 = ORIENTED_EDGE('',*,*,#2293,.T.) ;
#3069 = ORIENTED_EDGE('',*,*,#2294,.T.) ;
#3070 = ORIENTED_EDGE('',*,*,#2295,.T.) ;
#3071 = ORIENTED_EDGE('',*,*,#2296,.T.) ;
#3072 = ORIENTED_EDGE('',*,*,#2297,.T.) ;
#3073 = ORIENTED_EDGE('',*,*,#2298,.T.) ;
#3074 = ORIENTED_EDGE('',*,*,#2299,.T.) ;
#3075 = ORIENTED_EDGE('',*,*,#2300,.T.) ;
#3076 = ORIENTED_EDGE('',*,*,#2301,.T.) ;
#3077 = ORIENTED_EDGE('',*,*,#2302,.T.) ;
#3078 = ORIENTED_EDGE('',*,*,#2303,.T.) ;
#3079 = ORIENTED_EDGE('',*,*,#2304,.T.) ;
#3080 = ORIENTED_EDGE('',*,*,#2305,.T.) ;
#3081 = ORIENTED_EDGE('',*,*,#2306,.F.) ;
#3082 = ORIENTED_EDGE('',*,*,#2292,.F.) ;
#3083 = ORIENTED_EDGE('',*,*,#2306,.T.) ;
#3084 = ORIENTED_EDGE('',*,*,#2307,.T.) ;
#3085 = ORIENTED_EDGE('',*,*,#2308,.F.) ;
#3086 = ORIENTED_EDGE('',*,*,#2293,.F.) ;
#3087 = ORIENTED_EDGE('',*,*,#2308,.T.) ;
#3088 = ORIENTED_EDGE('',*,*,#2309,.T.) ;
#3089 = ORIENTED_EDGE('',*,*,#2310,.F.) ;
#3090 = ORIENTED_EDGE('',*,*,#2294,.F.) ;
#3091 = ORIENTED_EDGE('',*,*,#2310,.T.) ;
#3092 = ORIENTED_EDGE('',*,*,#2311,.T.) ;
#3093 = ORIENTED_EDGE('',*,*,#2312,.F.) ;
#3094 = ORIENTED_EDGE('',*,*,#2295,.F.) ;
#3095 = ORIENTED_EDGE('',*,*,#2312,.T.) ;
#3096 = ORIENTED_EDGE('',*,*,#2313,.T.) ;
#3097 = ORIENTED_EDGE('',*,*,#2314,.F.) ;
#3098 = ORIENTED_EDGE('',*,*,#2296,.F.) ;
#3099 = ORIENTED_EDGE('',*,*,#2314,.T.) ;
#3100 = ORIENTED_EDGE('',*,*,#2315,.T.) ;
#3101 = ORIENTED_EDGE('',*,*,#2316,.F.) ;
#3102 = ORIENTED_EDGE('',*,*,#2297,.F.) ;
#3103 = ORIENTED_EDGE('',*,*,#2316,.T.) ;
#3104 = ORIENTED_EDGE('',*,*,#2317,.T.) ;
#3105 = ORIENTED_EDGE('',*,*,#2318,.F.) ;
#3106 = ORIENTED_EDGE('',*,*,#2298,.F.) ;
#3107 = ORIENTED_EDGE('',*,*,#2318,.T.) ;
#3108 = ORIENTED_EDGE('',*,*,#2319,.T.) ;
#3109 = ORIENTED_EDGE('',*,*,#2320,.F.) ;
#3110 = ORIENTED_EDGE('',*,*,#2299,.F.) ;
#3111 = ORIENTED_EDGE('',*,*,#2320,.T.) ;
#3112 = ORIENTED_EDGE('',*,*,#2321,.T.) ;
#3113 = ORIENTED_EDGE('',*,*,#2322,.F.) ;
#3114 = ORIENTED_EDGE('',*,*,#2300,.F.) ;
#3115 = ORIENTED_EDGE('',*,*,#2322,.T.) ;
#3116 = ORIENTED_EDGE('',*,*,#2323,.T.) ;
#3117 = ORIENTED_EDGE('',*,*,#2324,.F.) ;
#3118 = ORIENTED_EDGE('',*,*,#2301,.F.) ;
#3119 = ORIENTED_EDGE('',*,*,#2324,.T.) ;
#3120 = ORIENTED_EDGE('',*,*,#2325,.T.) ;
#3121 = ORIENTED_EDGE('',*,*,#2326,.F.) ;
#3122 = ORIENTED_EDGE('',*,*,#2302,.F.) ;
#3123 = ORIENTED_EDGE('',*,*,#2303,.F.) ;
#3124 = ORIENTED_EDGE('',*,*,#2326,.T.) ;
#3125 = ORIENTED_EDGE('',*,*,#2327,.T.) ;
#3126 = ORIENTED_EDGE('',*,*,#2328,.T.) ;
#3127 = ORIENTED_EDGE('',*,*,#2329,.T.) ;
#3128 = ORIENTED_EDGE('',*,*,#2330,.T.) ;
#3129 = ORIENTED_EDGE('',*,*,#2304,.F.) ;
#3130 = ORIENTED_EDGE('',*,*,#2291,.F.) ;
#3131 = ORIENTED_EDGE('',*,*,#2331,.F.) ;
#3132 = ORIENTED_EDGE('',*,*,#2332,.F.) ;
#3133 = ORIENTED_EDGE('',*,*,#2333,.F.) ;
#3134 = ORIENTED_EDGE('',*,*,#2334,.F.) ;
#3135 = ORIENTED_EDGE('',*,*,#2335,.F.) ;
#3136 = ORIENTED_EDGE('',*,*,#2336,.F.) ;
#3137 = ORIENTED_EDGE('',*,*,#2337,.F.) ;
#3138 = ORIENTED_EDGE('',*,*,#2338,.F.) ;
#3139 = ORIENTED_EDGE('',*,*,#2339,.F.) ;
#3140 = ORIENTED_EDGE('',*,*,#2340,.F.) ;
#3141 = ORIENTED_EDGE('',*,*,#2341,.F.) ;
#3142 = ORIENTED_EDGE('',*,*,#2342,.F.) ;
#3143 = ORIENTED_EDGE('',*,*,#2343,.F.) ;
#3144 = ORIENTED_EDGE('',*,*,#2344,.F.) ;
#3145 = ORIENTED_EDGE('',*,*,#2282,.F.) ;
#3146 = ORIENTED_EDGE('',*,*,#2345,.F.) ;
#3147 = ORIENTED_EDGE('',*,*,#2346,.T.) ;
#3148 = ORIENTED_EDGE('',*,*,#2347,.F.) ;
#3149 = ORIENTED_EDGE('',*,*,#2321,.F.) ;
#3150 = ORIENTED_EDGE('',*,*,#2348,.T.) ;
#3151 = ORIENTED_EDGE('',*,*,#2349,.T.) ;
#3152 = ORIENTED_EDGE('',*,*,#2313,.F.) ;
#3153 = ORIENTED_EDGE('',*,*,#2350,.F.) ;
#3154 = ORIENTED_EDGE('',*,*,#2351,.T.) ;
#3155 = ORIENTED_EDGE('',*,*,#2350,.T.) ;
#3156 = ORIENTED_EDGE('',*,*,#2311,.F.) ;
#3157 = ORIENTED_EDGE('',*,*,#2352,.T.) ;
#3158 = ORIENTED_EDGE('',*,*,#2353,.T.) ;
#3159 = ORIENTED_EDGE('',*,*,#2354,.T.) ;
#3160 = ORIENTED_EDGE('',*,*,#2348,.F.) ;
#3161 = ORIENTED_EDGE('',*,*,#2319,.F.) ;
#3162 = ORIENTED_EDGE('',*,*,#2355,.F.) ;
#3163 = ORIENTED_EDGE('',*,*,#2355,.T.) ;
#3164 = ORIENTED_EDGE('',*,*,#2317,.F.) ;
#3165 = ORIENTED_EDGE('',*,*,#2356,.F.) ;
#3166 = ORIENTED_EDGE('',*,*,#2357,.T.) ;
#3167 = ORIENTED_EDGE('',*,*,#2356,.T.) ;
#3168 = ORIENTED_EDGE('',*,*,#2315,.F.) ;
#3169 = ORIENTED_EDGE('',*,*,#2349,.F.) ;
#3170 = ORIENTED_EDGE('',*,*,#2358,.T.) ;
#3171 = ORIENTED_EDGE('',*,*,#2359,.T.) ;
#3172 = ORIENTED_EDGE('',*,*,#2352,.F.) ;
#3173 = ORIENTED_EDGE('',*,*,#2309,.F.) ;
#3174 = ORIENTED_EDGE('',*,*,#2360,.T.) ;
#3175 = ORIENTED_EDGE('',*,*,#2345,.T.) ;
#3176 = ORIENTED_EDGE('',*,*,#2281,.F.) ;
#3177 = ORIENTED_EDGE('',*,*,#2285,.T.) ;
#3178 = ORIENTED_EDGE('',*,*,#2287,.F.) ;
#3179 = ORIENTED_EDGE('',*,*,#2289,.F.) ;
#3180 = ORIENTED_EDGE('',*,*,#2328,.F.) ;
#3181 = ORIENTED_EDGE('',*,*,#2361,.F.) ;
#3182 = ORIENTED_EDGE('',*,*,#2362,.F.) ;
#3183 = ORIENTED_EDGE('',*,*,#2363,.F.) ;
#3184 = ORIENTED_EDGE('',*,*,#2364,.F.) ;
#3185 = ORIENTED_EDGE('',*,*,#2365,.T.) ;
#3186 = ORIENTED_EDGE('',*,*,#2329,.F.) ;
#3187 = ORIENTED_EDGE('',*,*,#2290,.F.) ;
#3188 = ORIENTED_EDGE('',*,*,#2288,.F.) ;
#3189 = ORIENTED_EDGE('',*,*,#2283,.F.) ;
#3190 = ORIENTED_EDGE('',*,*,#2279,.F.) ;
#3191 = ORIENTED_EDGE('',*,*,#2344,.T.) ;
#3192 = ORIENTED_EDGE('',*,*,#2366,.F.) ;
#3193 = ORIENTED_EDGE('',*,*,#2367,.F.) ;
#3194 = ORIENTED_EDGE('',*,*,#2368,.F.) ;
#3195 = ORIENTED_EDGE('',*,*,#2369,.T.) ;
#3196 = ORIENTED_EDGE('',*,*,#2361,.T.) ;
#3197 = ORIENTED_EDGE('',*,*,#2327,.F.) ;
#3198 = ORIENTED_EDGE('',*,*,#2370,.F.) ;
#3199 = ORIENTED_EDGE('',*,*,#2370,.T.) ;
#3200 = ORIENTED_EDGE('',*,*,#2325,.F.) ;
#3201 = ORIENTED_EDGE('',*,*,#2371,.F.) ;
#3202 = ORIENTED_EDGE('',*,*,#2372,.T.) ;
#3203 = ORIENTED_EDGE('',*,*,#2373,.T.) ;
#3204 = ORIENTED_EDGE('',*,*,#2330,.F.) ;
#3205 = ORIENTED_EDGE('',*,*,#2365,.F.) ;
#3206 = ORIENTED_EDGE('',*,*,#2374,.T.) ;
#3207 = ORIENTED_EDGE('',*,*,#2375,.T.) ;
#3208 = ORIENTED_EDGE('',*,*,#2305,.F.) ;
#3209 = ORIENTED_EDGE('',*,*,#2373,.F.) ;
#3210 = ORIENTED_EDGE('',*,*,#2376,.T.) ;
#3211 = ORIENTED_EDGE('',*,*,#2377,.T.) ;
#3212 = ORIENTED_EDGE('',*,*,#2342,.T.) ;
#3213 = ORIENTED_EDGE('',*,*,#2378,.F.) ;
#3214 = ORIENTED_EDGE('',*,*,#2376,.F.) ;
#3215 = ORIENTED_EDGE('',*,*,#2378,.T.) ;
#3216 = ORIENTED_EDGE('',*,*,#2341,.T.) ;
#3217 = ORIENTED_EDGE('',*,*,#2379,.F.) ;
#3218 = ORIENTED_EDGE('',*,*,#2380,.F.) ;
#3219 = ORIENTED_EDGE('',*,*,#2379,.T.) ;
#3220 = ORIENTED_EDGE('',*,*,#2340,.T.) ;
#3221 = ORIENTED_EDGE('',*,*,#2381,.F.) ;
#3222 = ORIENTED_EDGE('',*,*,#2359,.F.) ;
#3223 = ORIENTED_EDGE('',*,*,#2381,.T.) ;
#3224 = ORIENTED_EDGE('',*,*,#2339,.T.) ;
#3225 = ORIENTED_EDGE('',*,*,#2382,.F.) ;
#3226 = ORIENTED_EDGE('',*,*,#2353,.F.) ;
#3227 = ORIENTED_EDGE('',*,*,#2382,.T.) ;
#3228 = ORIENTED_EDGE('',*,*,#2338,.T.) ;
#3229 = ORIENTED_EDGE('',*,*,#2383,.F.) ;
#3230 = ORIENTED_EDGE('',*,*,#2351,.F.) ;
#3231 = ORIENTED_EDGE('',*,*,#2383,.T.) ;
#3232 = ORIENTED_EDGE('',*,*,#2337,.T.) ;
#3233 = ORIENTED_EDGE('',*,*,#2384,.F.) ;
#3234 = ORIENTED_EDGE('',*,*,#2358,.F.) ;
#3235 = ORIENTED_EDGE('',*,*,#2384,.T.) ;
#3236 = ORIENTED_EDGE('',*,*,#2336,.T.) ;
#3237 = ORIENTED_EDGE('',*,*,#2385,.F.) ;
#3238 = ORIENTED_EDGE('',*,*,#2357,.F.) ;
#3239 = ORIENTED_EDGE('',*,*,#2385,.T.) ;
#3240 = ORIENTED_EDGE('',*,*,#2335,.T.) ;
#3241 = ORIENTED_EDGE('',*,*,#2386,.F.) ;
#3242 = ORIENTED_EDGE('',*,*,#2354,.F.) ;
#3243 = ORIENTED_EDGE('',*,*,#2386,.T.) ;
#3244 = ORIENTED_EDGE('',*,*,#2334,.T.) ;
#3245 = ORIENTED_EDGE('',*,*,#2387,.F.) ;
#3246 = ORIENTED_EDGE('',*,*,#2346,.F.) ;
#3247 = ORIENTED_EDGE('',*,*,#2387,.T.) ;
#3248 = ORIENTED_EDGE('',*,*,#2333,.T.) ;
#3249 = ORIENTED_EDGE('',*,*,#2388,.F.) ;
#3250 = ORIENTED_EDGE('',*,*,#2389,.F.) ;
#3251 = ORIENTED_EDGE('',*,*,#2388,.T.) ;
#3252 = ORIENTED_EDGE('',*,*,#2332,.T.) ;
#3253 = ORIENTED_EDGE('',*,*,#2390,.F.) ;
#3254 = ORIENTED_EDGE('',*,*,#2372,.F.) ;
#3255 = ORIENTED_EDGE('',*,*,#2362,.T.) ;
#3256 = ORIENTED_EDGE('',*,*,#2369,.F.) ;
#3257 = ORIENTED_EDGE('',*,*,#2390,.T.) ;
#3258 = ORIENTED_EDGE('',*,*,#2331,.T.) ;
#3259 = ORIENTED_EDGE('',*,*,#2343,.T.) ;
#3260 = ORIENTED_EDGE('',*,*,#2377,.F.) ;
#3261 = ORIENTED_EDGE('',*,*,#2374,.F.) ;
#3262 = ORIENTED_EDGE('',*,*,#2366,.T.) ;
#3263 = ORIENTED_EDGE('',*,*,#2391,.T.) ;
#3264 = ORIENTED_EDGE('',*,*,#2392,.T.) ;
#3265 = ORIENTED_EDGE('',*,*,#2368,.T.) ;
#3266 = ORIENTED_EDGE('',*,*,#2392,.F.) ;
#3267 = ORIENTED_EDGE('',*,*,#2393,.T.) ;
#3268 = ORIENTED_EDGE('',*,*,#2391,.F.) ;
#3269 = ORIENTED_EDGE('',*,*,#2394,.T.) ;
#3270 = ORIENTED_EDGE('',*,*,#2395,.T.) ;
#3271 = ORIENTED_EDGE('',*,*,#2394,.F.) ;
#3272 = ORIENTED_EDGE('',*,*,#2393,.F.) ;
#3273 = ORIENTED_EDGE('',*,*,#2396,.T.) ;
#3274 = ORIENTED_EDGE('',*,*,#2397,.T.) ;
#3275 = ORIENTED_EDGE('',*,*,#2367,.T.) ;
#3276 = ORIENTED_EDGE('',*,*,#2397,.F.) ;
#3277 = ORIENTED_EDGE('',*,*,#2398,.T.) ;
#3278 = ORIENTED_EDGE('',*,*,#2360,.F.) ;
#3279 = ORIENTED_EDGE('',*,*,#2307,.F.) ;
#3280 = ORIENTED_EDGE('',*,*,#2375,.F.) ;
#3281 = ORIENTED_EDGE('',*,*,#2380,.T.) ;
#3282 = ORIENTED_EDGE('',*,*,#2399,.F.) ;
#3283 = ORIENTED_EDGE('',*,*,#2395,.F.) ;
#3284 = ORIENTED_EDGE('',*,*,#2396,.F.) ;
#3285 = ORIENTED_EDGE('',*,*,#2400,.T.) ;
#3286 = ORIENTED_EDGE('',*,*,#2399,.T.) ;
#3287 = ORIENTED_EDGE('',*,*,#2400,.F.) ;
#3288 = ORIENTED_EDGE('',*,*,#2398,.F.) ;
#3289 = ORIENTED_EDGE('',*,*,#2401,.T.) ;
#3290 = ORIENTED_EDGE('',*,*,#2402,.T.) ;
#3291 = ORIENTED_EDGE('',*,*,#2364,.T.) ;
#3292 = ORIENTED_EDGE('',*,*,#2402,.F.) ;
#3293 = ORIENTED_EDGE('',*,*,#2403,.T.) ;
#3294 = ORIENTED_EDGE('',*,*,#2401,.F.) ;
#3295 = ORIENTED_EDGE('',*,*,#2404,.T.) ;
#3296 = ORIENTED_EDGE('',*,*,#2405,.T.) ;
#3297 = ORIENTED_EDGE('',*,*,#2404,.F.) ;
#3298 = ORIENTED_EDGE('',*,*,#2403,.F.) ;
#3299 = ORIENTED_EDGE('',*,*,#2406,.T.) ;
#3300 = ORIENTED_EDGE('',*,*,#2407,.T.) ;
#3301 = ORIENTED_EDGE('',*,*,#2363,.T.) ;
#3302 = ORIENTED_EDGE('',*,*,#2407,.F.) ;
#3303 = ORIENTED_EDGE('',*,*,#2408,.T.) ;
#3304 = ORIENTED_EDGE('',*,*,#2371,.T.) ;
#3305 = ORIENTED_EDGE('',*,*,#2323,.F.) ;
#3306 = ORIENTED_EDGE('',*,*,#2347,.T.) ;
#3307 = ORIENTED_EDGE('',*,*,#2389,.T.) ;
#3308 = ORIENTED_EDGE('',*,*,#2409,.F.) ;
#3309 = ORIENTED_EDGE('',*,*,#2405,.F.) ;
#3310 = ORIENTED_EDGE('',*,*,#2406,.F.) ;
#3311 = ORIENTED_EDGE('',*,*,#2410,.T.) ;
#3312 = ORIENTED_EDGE('',*,*,#2409,.T.) ;
#3313 = ORIENTED_EDGE('',*,*,#2410,.F.) ;
#3314 = ORIENTED_EDGE('',*,*,#2408,.F.) ;
#3315 = ORIENTED_EDGE('',*,*,#2411,.F.) ;
#3316 = ORIENTED_EDGE('',*,*,#2412,.T.) ;
#3317 = ORIENTED_EDGE('',*,*,#2413,.T.) ;
#3318 = ORIENTED_EDGE('',*,*,#2412,.F.) ;
#3319 = ORIENTED_EDGE('',*,*,#2414,.F.) ;
#3320 = ORIENTED_EDGE('',*,*,#2415,.T.) ;
#3321 = ORIENTED_EDGE('',*,*,#2416,.T.) ;
#3322 = ORIENTED_EDGE('',*,*,#2415,.F.) ;
#3323 = ORIENTED_EDGE('',*,*,#2413,.F.) ;
#3324 = ORIENTED_EDGE('',*,*,#2414,.T.) ;
#3325 = ORIENTED_EDGE('',*,*,#2411,.T.) ;
#3326 = ORIENTED_EDGE('',*,*,#2416,.F.) ;
#3327 = ORIENTED_EDGE('',*,*,#2417,.F.) ;
#3328 = ORIENTED_EDGE('',*,*,#2418,.T.) ;
#3329 = ORIENTED_EDGE('',*,*,#2419,.T.) ;
#3330 = ORIENTED_EDGE('',*,*,#2418,.F.) ;
#3331 = ORIENTED_EDGE('',*,*,#2420,.F.) ;
#3332 = ORIENTED_EDGE('',*,*,#2421,.T.) ;
#3333 = ORIENTED_EDGE('',*,*,#2422,.T.) ;
#3334 = ORIENTED_EDGE('',*,*,#2421,.F.) ;
#3335 = ORIENTED_EDGE('',*,*,#2419,.F.) ;
#3336 = ORIENTED_EDGE('',*,*,#2420,.T.) ;
#3337 = ORIENTED_EDGE('',*,*,#2417,.T.) ;
#3338 = ORIENTED_EDGE('',*,*,#2422,.F.) ;
#3339 = ORIENTED_EDGE('',*,*,#2423,.F.) ;
#3340 = ORIENTED_EDGE('',*,*,#2424,.T.) ;
#3341 = ORIENTED_EDGE('',*,*,#2425,.T.) ;
#3342 = ORIENTED_EDGE('',*,*,#2424,.F.) ;
#3343 = ORIENTED_EDGE('',*,*,#2426,.F.) ;
#3344 = ORIENTED_EDGE('',*,*,#2427,.T.) ;
#3345 = ORIENTED_EDGE('',*,*,#2428,.T.) ;
#3346 = ORIENTED_EDGE('',*,*,#2427,.F.) ;
#3347 = ORIENTED_EDGE('',*,*,#2425,.F.) ;
#3348 = ORIENTED_EDGE('',*,*,#2426,.T.) ;
#3349 = ORIENTED_EDGE('',*,*,#2423,.T.) ;
#3350 = ORIENTED_EDGE('',*,*,#2428,.F.) ;
#3351 = ORIENTED_EDGE('',*,*,#2429,.F.) ;
#3352 = ORIENTED_EDGE('',*,*,#2430,.T.) ;
#3353 = ORIENTED_EDGE('',*,*,#2431,.T.) ;
#3354 = ORIENTED_EDGE('',*,*,#2430,.F.) ;
#3355 = ORIENTED_EDGE('',*,*,#2432,.F.) ;
#3356 = ORIENTED_EDGE('',*,*,#2433,.T.) ;
#3357 = ORIENTED_EDGE('',*,*,#2434,.T.) ;
#3358 = ORIENTED_EDGE('',*,*,#2433,.F.) ;
#3359 = ORIENTED_EDGE('',*,*,#2431,.F.) ;
#3360 = ORIENTED_EDGE('',*,*,#2432,.T.) ;
#3361 = ORIENTED_EDGE('',*,*,#2429,.T.) ;
#3362 = ORIENTED_EDGE('',*,*,#2434,.F.) ;
#3363 = ORIENTED_EDGE('',*,*,#2435,.F.) ;
#3364 = ORIENTED_EDGE('',*,*,#2436,.T.) ;
#3365 = ORIENTED_EDGE('',*,*,#2437,.T.) ;
#3366 = ORIENTED_EDGE('',*,*,#2438,.F.) ;
#3367 = ORIENTED_EDGE('',*,*,#2439,.F.) ;
#3368 = ORIENTED_EDGE('',*,*,#2440,.T.) ;
#3369 = ORIENTED_EDGE('',*,*,#2435,.T.) ;
#3370 = ORIENTED_EDGE('',*,*,#2441,.F.) ;
#3371 = ORIENTED_EDGE('',*,*,#2437,.F.) ;
#3372 = ORIENTED_EDGE('',*,*,#2442,.T.) ;
#3373 = ORIENTED_EDGE('',*,*,#2443,.T.) ;
#3374 = ORIENTED_EDGE('',*,*,#2444,.F.) ;
#3375 = ORIENTED_EDGE('',*,*,#2438,.T.) ;
#3376 = ORIENTED_EDGE('',*,*,#2444,.T.) ;
#3377 = ORIENTED_EDGE('',*,*,#2445,.T.) ;
#3378 = ORIENTED_EDGE('',*,*,#2446,.T.) ;
#3379 = ORIENTED_EDGE('',*,*,#2447,.T.) ;
#3380 = ORIENTED_EDGE('',*,*,#2441,.T.) ;
#3381 = ORIENTED_EDGE('',*,*,#2448,.F.) ;
#3382 = ORIENTED_EDGE('',*,*,#2449,.T.) ;
#3383 = ORIENTED_EDGE('',*,*,#2439,.T.) ;
#3384 = ORIENTED_EDGE('',*,*,#2447,.F.) ;
#3385 = ORIENTED_EDGE('',*,*,#2443,.F.) ;
#3386 = ORIENTED_EDGE('',*,*,#2450,.T.) ;
#3387 = ORIENTED_EDGE('',*,*,#2451,.T.) ;
#3388 = ORIENTED_EDGE('',*,*,#2445,.F.) ;
#3389 = ORIENTED_EDGE('',*,*,#2451,.F.) ;
#3390 = ORIENTED_EDGE('',*,*,#2452,.T.) ;
#3391 = ORIENTED_EDGE('',*,*,#2448,.T.) ;
#3392 = ORIENTED_EDGE('',*,*,#2446,.F.) ;
#3393 = ORIENTED_EDGE('',*,*,#2453,.T.) ;
#3394 = ORIENTED_EDGE('',*,*,#2449,.F.) ;
#3395 = ORIENTED_EDGE('',*,*,#2452,.F.) ;
#3396 = ORIENTED_EDGE('',*,*,#2450,.F.) ;
#3397 = ORIENTED_EDGE('',*,*,#2442,.F.) ;
#3398 = ORIENTED_EDGE('',*,*,#2436,.F.) ;
#3399 = ORIENTED_EDGE('',*,*,#2440,.F.) ;
#3400 = ORIENTED_EDGE('',*,*,#2454,.F.) ;
#3401 = ORIENTED_EDGE('',*,*,#2455,.T.) ;
#3402 = ORIENTED_EDGE('',*,*,#2456,.F.) ;
#3403 = ORIENTED_EDGE('',*,*,#2453,.F.) ;
#3404 = ORIENTED_EDGE('',*,*,#2457,.T.) ;
#3405 = ORIENTED_EDGE('',*,*,#2458,.T.) ;
#3406 = ORIENTED_EDGE('',*,*,#2457,.F.) ;
#3407 = ORIENTED_EDGE('',*,*,#2458,.F.) ;
#3408 = ORIENTED_EDGE('',*,*,#2459,.T.) ;
#3409 = ORIENTED_EDGE('',*,*,#2454,.T.) ;
#3410 = ORIENTED_EDGE('',*,*,#2459,.F.) ;
#3411 = ORIENTED_EDGE('',*,*,#2455,.F.) ;
#3412 = ORIENTED_EDGE('',*,*,#2460,.T.) ;
#3413 = ORIENTED_EDGE('',*,*,#2461,.T.) ;
#3414 = ORIENTED_EDGE('',*,*,#2460,.F.) ;
#3415 = ORIENTED_EDGE('',*,*,#2461,.F.) ;
#3416 = ORIENTED_EDGE('',*,*,#2462,.T.) ;
#3417 = ORIENTED_EDGE('',*,*,#2463,.T.) ;
#3418 = ORIENTED_EDGE('',*,*,#2462,.F.) ;
#3419 = ORIENTED_EDGE('',*,*,#2463,.F.) ;
#3420 = ORIENTED_EDGE('',*,*,#2464,.T.) ;
#3421 = ORIENTED_EDGE('',*,*,#2456,.T.) ;
#3422 = ORIENTED_EDGE('',*,*,#2464,.F.) ;
#3423 = ORIENTED_EDGE('',*,*,#2465,.F.) ;
#3424 = ORIENTED_EDGE('',*,*,#2466,.T.) ;
#3425 = ORIENTED_EDGE('',*,*,#2467,.T.) ;
#3426 = ORIENTED_EDGE('',*,*,#2468,.F.) ;
#3427 = ORIENTED_EDGE('',*,*,#2469,.F.) ;
#3428 = ORIENTED_EDGE('',*,*,#2470,.T.) ;
#3429 = ORIENTED_EDGE('',*,*,#2465,.T.) ;
#3430 = ORIENTED_EDGE('',*,*,#2471,.F.) ;
#3431 = ORIENTED_EDGE('',*,*,#2467,.F.) ;
#3432 = ORIENTED_EDGE('',*,*,#2472,.T.) ;
#3433 = ORIENTED_EDGE('',*,*,#2473,.T.) ;
#3434 = ORIENTED_EDGE('',*,*,#2474,.F.) ;
#3435 = ORIENTED_EDGE('',*,*,#2468,.T.) ;
#3436 = ORIENTED_EDGE('',*,*,#2474,.T.) ;
#3437 = ORIENTED_EDGE('',*,*,#2475,.T.) ;
#3438 = ORIENTED_EDGE('',*,*,#2476,.T.) ;
#3439 = ORIENTED_EDGE('',*,*,#2477,.T.) ;
#3440 = ORIENTED_EDGE('',*,*,#2471,.T.) ;
#3441 = ORIENTED_EDGE('',*,*,#2478,.F.) ;
#3442 = ORIENTED_EDGE('',*,*,#2479,.T.) ;
#3443 = ORIENTED_EDGE('',*,*,#2469,.T.) ;
#3444 = ORIENTED_EDGE('',*,*,#2477,.F.) ;
#3445 = ORIENTED_EDGE('',*,*,#2473,.F.) ;
#3446 = ORIENTED_EDGE('',*,*,#2480,.T.) ;
#3447 = ORIENTED_EDGE('',*,*,#2481,.T.) ;
#3448 = ORIENTED_EDGE('',*,*,#2475,.F.) ;
#3449 = ORIENTED_EDGE('',*,*,#2481,.F.) ;
#3450 = ORIENTED_EDGE('',*,*,#2482,.T.) ;
#3451 = ORIENTED_EDGE('',*,*,#2478,.T.) ;
#3452 = ORIENTED_EDGE('',*,*,#2476,.F.) ;
#3453 = ORIENTED_EDGE('',*,*,#2483,.T.) ;
#3454 = ORIENTED_EDGE('',*,*,#2479,.F.) ;
#3455 = ORIENTED_EDGE('',*,*,#2482,.F.) ;
#3456 = ORIENTED_EDGE('',*,*,#2480,.F.) ;
#3457 = ORIENTED_EDGE('',*,*,#2472,.F.) ;
#3458 = ORIENTED_EDGE('',*,*,#2466,.F.) ;
#3459 = ORIENTED_EDGE('',*,*,#2470,.F.) ;
#3460 = ORIENTED_EDGE('',*,*,#2484,.F.) ;
#3461 = ORIENTED_EDGE('',*,*,#2485,.T.) ;
#3462 = ORIENTED_EDGE('',*,*,#2486,.F.) ;
#3463 = ORIENTED_EDGE('',*,*,#2483,.F.) ;
#3464 = ORIENTED_EDGE('',*,*,#2487,.T.) ;
#3465 = ORIENTED_EDGE('',*,*,#2488,.T.) ;
#3466 = ORIENTED_EDGE('',*,*,#2487,.F.) ;
#3467 = ORIENTED_EDGE('',*,*,#2488,.F.) ;
#3468 = ORIENTED_EDGE('',*,*,#2489,.T.) ;
#3469 = ORIENTED_EDGE('',*,*,#2484,.T.) ;
#3470 = ORIENTED_EDGE('',*,*,#2489,.F.) ;
#3471 = ORIENTED_EDGE('',*,*,#2485,.F.) ;
#3472 = ORIENTED_EDGE('',*,*,#2490,.T.) ;
#3473 = ORIENTED_EDGE('',*,*,#2491,.T.) ;
#3474 = ORIENTED_EDGE('',*,*,#2490,.F.) ;
#3475 = ORIENTED_EDGE('',*,*,#2491,.F.) ;
#3476 = ORIENTED_EDGE('',*,*,#2492,.T.) ;
#3477 = ORIENTED_EDGE('',*,*,#2493,.T.) ;
#3478 = ORIENTED_EDGE('',*,*,#2492,.F.) ;
#3479 = ORIENTED_EDGE('',*,*,#2493,.F.) ;
#3480 = ORIENTED_EDGE('',*,*,#2494,.T.) ;
#3481 = ORIENTED_EDGE('',*,*,#2486,.T.) ;
#3482 = ORIENTED_EDGE('',*,*,#2494,.F.) ;
#3483 = ORIENTED_EDGE('',*,*,#2495,.F.) ;
#3484 = ORIENTED_EDGE('',*,*,#2496,.T.) ;
#3485 = ORIENTED_EDGE('',*,*,#2497,.T.) ;
#3486 = ORIENTED_EDGE('',*,*,#2498,.F.) ;
#3487 = ORIENTED_EDGE('',*,*,#2499,.F.) ;
#3488 = ORIENTED_EDGE('',*,*,#2500,.T.) ;
#3489 = ORIENTED_EDGE('',*,*,#2495,.T.) ;
#3490 = ORIENTED_EDGE('',*,*,#2501,.F.) ;
#3491 = ORIENTED_EDGE('',*,*,#2497,.F.) ;
#3492 = ORIENTED_EDGE('',*,*,#2502,.T.) ;
#3493 = ORIENTED_EDGE('',*,*,#2503,.T.) ;
#3494 = ORIENTED_EDGE('',*,*,#2504,.F.) ;
#3495 = ORIENTED_EDGE('',*,*,#2498,.T.) ;
#3496 = ORIENTED_EDGE('',*,*,#2504,.T.) ;
#3497 = ORIENTED_EDGE('',*,*,#2505,.T.) ;
#3498 = ORIENTED_EDGE('',*,*,#2506,.T.) ;
#3499 = ORIENTED_EDGE('',*,*,#2507,.T.) ;
#3500 = ORIENTED_EDGE('',*,*,#2501,.T.) ;
#3501 = ORIENTED_EDGE('',*,*,#2508,.F.) ;
#3502 = ORIENTED_EDGE('',*,*,#2509,.T.) ;
#3503 = ORIENTED_EDGE('',*,*,#2499,.T.) ;
#3504 = ORIENTED_EDGE('',*,*,#2507,.F.) ;
#3505 = ORIENTED_EDGE('',*,*,#2503,.F.) ;
#3506 = ORIENTED_EDGE('',*,*,#2510,.T.) ;
#3507 = ORIENTED_EDGE('',*,*,#2511,.T.) ;
#3508 = ORIENTED_EDGE('',*,*,#2505,.F.) ;
#3509 = ORIENTED_EDGE('',*,*,#2511,.F.) ;
#3510 = ORIENTED_EDGE('',*,*,#2512,.T.) ;
#3511 = ORIENTED_EDGE('',*,*,#2508,.T.) ;
#3512 = ORIENTED_EDGE('',*,*,#2506,.F.) ;
#3513 = ORIENTED_EDGE('',*,*,#2513,.T.) ;
#3514 = ORIENTED_EDGE('',*,*,#2509,.F.) ;
#3515 = ORIENTED_EDGE('',*,*,#2512,.F.) ;
#3516 = ORIENTED_EDGE('',*,*,#2510,.F.) ;
#3517 = ORIENTED_EDGE('',*,*,#2502,.F.) ;
#3518 = ORIENTED_EDGE('',*,*,#2496,.F.) ;
#3519 = ORIENTED_EDGE('',*,*,#2500,.F.) ;
#3520 = ORIENTED_EDGE('',*,*,#2514,.F.) ;
#3521 = ORIENTED_EDGE('',*,*,#2515,.T.) ;
#3522 = ORIENTED_EDGE('',*,*,#2516,.F.) ;
#3523 = ORIENTED_EDGE('',*,*,#2513,.F.) ;
#3524 = ORIENTED_EDGE('',*,*,#2517,.T.) ;
#3525 = ORIENTED_EDGE('',*,*,#2518,.T.) ;
#3526 = ORIENTED_EDGE('',*,*,#2517,.F.) ;
#3527 = ORIENTED_EDGE('',*,*,#2518,.F.) ;
#3528 = ORIENTED_EDGE('',*,*,#2519,.T.) ;
#3529 = ORIENTED_EDGE('',*,*,#2514,.T.) ;
#3530 = ORIENTED_EDGE('',*,*,#2519,.F.) ;
#3531 = ORIENTED_EDGE('',*,*,#2515,.F.) ;
#3532 = ORIENTED_EDGE('',*,*,#2520,.T.) ;
#3533 = ORIENTED_EDGE('',*,*,#2521,.T.) ;
#3534 = ORIENTED_EDGE('',*,*,#2520,.F.) ;
#3535 = ORIENTED_EDGE('',*,*,#2521,.F.) ;
#3536 = ORIENTED_EDGE('',*,*,#2522,.T.) ;
#3537 = ORIENTED_EDGE('',*,*,#2523,.T.) ;
#3538 = ORIENTED_EDGE('',*,*,#2522,.F.) ;
#3539 = ORIENTED_EDGE('',*,*,#2523,.F.) ;
#3540 = ORIENTED_EDGE('',*,*,#2524,.T.) ;
#3541 = ORIENTED_EDGE('',*,*,#2516,.T.) ;
#3542 = ORIENTED_EDGE('',*,*,#2524,.F.) ;
#3543 = ORIENTED_EDGE('',*,*,#2525,.F.) ;
#3544 = ORIENTED_EDGE('',*,*,#2526,.T.) ;
#3545 = ORIENTED_EDGE('',*,*,#2527,.T.) ;
#3546 = ORIENTED_EDGE('',*,*,#2528,.F.) ;
#3547 = ORIENTED_EDGE('',*,*,#2529,.F.) ;
#3548 = ORIENTED_EDGE('',*,*,#2530,.T.) ;
#3549 = ORIENTED_EDGE('',*,*,#2525,.T.) ;
#3550 = ORIENTED_EDGE('',*,*,#2531,.F.) ;
#3551 = ORIENTED_EDGE('',*,*,#2527,.F.) ;
#3552 = ORIENTED_EDGE('',*,*,#2532,.T.) ;
#3553 = ORIENTED_EDGE('',*,*,#2533,.T.) ;
#3554 = ORIENTED_EDGE('',*,*,#2534,.F.) ;
#3555 = ORIENTED_EDGE('',*,*,#2528,.T.) ;
#3556 = ORIENTED_EDGE('',*,*,#2534,.T.) ;
#3557 = ORIENTED_EDGE('',*,*,#2535,.T.) ;
#3558 = ORIENTED_EDGE('',*,*,#2536,.T.) ;
#3559 = ORIENTED_EDGE('',*,*,#2537,.T.) ;
#3560 = ORIENTED_EDGE('',*,*,#2531,.T.) ;
#3561 = ORIENTED_EDGE('',*,*,#2538,.F.) ;
#3562 = ORIENTED_EDGE('',*,*,#2539,.T.) ;
#3563 = ORIENTED_EDGE('',*,*,#2529,.T.) ;
#3564 = ORIENTED_EDGE('',*,*,#2537,.F.) ;
#3565 = ORIENTED_EDGE('',*,*,#2533,.F.) ;
#3566 = ORIENTED_EDGE('',*,*,#2540,.T.) ;
#3567 = ORIENTED_EDGE('',*,*,#2541,.T.) ;
#3568 = ORIENTED_EDGE('',*,*,#2535,.F.) ;
#3569 = ORIENTED_EDGE('',*,*,#2541,.F.) ;
#3570 = ORIENTED_EDGE('',*,*,#2542,.T.) ;
#3571 = ORIENTED_EDGE('',*,*,#2538,.T.) ;
#3572 = ORIENTED_EDGE('',*,*,#2536,.F.) ;
#3573 = ORIENTED_EDGE('',*,*,#2543,.T.) ;
#3574 = ORIENTED_EDGE('',*,*,#2539,.F.) ;
#3575 = ORIENTED_EDGE('',*,*,#2542,.F.) ;
#3576 = ORIENTED_EDGE('',*,*,#2540,.F.) ;
#3577 = ORIENTED_EDGE('',*,*,#2532,.F.) ;
#3578 = ORIENTED_EDGE('',*,*,#2526,.F.) ;
#3579 = ORIENTED_EDGE('',*,*,#2530,.F.) ;
#3580 = ORIENTED_EDGE('',*,*,#2544,.F.) ;
#3581 = ORIENTED_EDGE('',*,*,#2545,.T.) ;
#3582 = ORIENTED_EDGE('',*,*,#2546,.F.) ;
#3583 = ORIENTED_EDGE('',*,*,#2543,.F.) ;
#3584 = ORIENTED_EDGE('',*,*,#2547,.T.) ;
#3585 = ORIENTED_EDGE('',*,*,#2548,.T.) ;
#3586 = ORIENTED_EDGE('',*,*,#2547,.F.) ;
#3587 = ORIENTED_EDGE('',*,*,#2548,.F.) ;
#3588 = ORIENTED_EDGE('',*,*,#2549,.T.) ;
#3589 = ORIENTED_EDGE('',*,*,#2544,.T.) ;
#3590 = ORIENTED_EDGE('',*,*,#2549,.F.) ;
#3591 = ORIENTED_EDGE('',*,*,#2545,.F.) ;
#3592 = ORIENTED_EDGE('',*,*,#2550,.T.) ;
#3593 = ORIENTED_EDGE('',*,*,#2551,.T.) ;
#3594 = ORIENTED_EDGE('',*,*,#2550,.F.) ;
#3595 = ORIENTED_EDGE('',*,*,#2551,.F.) ;
#3596 = ORIENTED_EDGE('',*,*,#2552,.T.) ;
#3597 = ORIENTED_EDGE('',*,*,#2553,.T.) ;
#3598 = ORIENTED_EDGE('',*,*,#2552,.F.) ;
#3599 = ORIENTED_EDGE('',*,*,#2553,.F.) ;
#3600 = ORIENTED_EDGE('',*,*,#2554,.T.) ;
#3601 = ORIENTED_EDGE('',*,*,#2546,.T.) ;
#3602 = ORIENTED_EDGE('',*,*,#2554,.F.) ;
#3603 = CYLINDRICAL_SURFACE('',#4018,27.5) ;
#3604 = CYLINDRICAL_SURFACE('',#4025,3.25) ;
#3605 = CYLINDRICAL_SURFACE('',#4030,3.25) ;
#3606 = CYLINDRICAL_SURFACE('',#4035,3.25) ;
#3607 = CYLINDRICAL_SURFACE('',#4040,3.25) ;
#3608 = CYLINDRICAL_SURFACE('',#4108,0.8) ;
#3609 = CYLINDRICAL_SURFACE('',#4110,0.8) ;
#3610 = CYLINDRICAL_SURFACE('',#4112,0.8) ;
#3611 = CYLINDRICAL_SURFACE('',#4114,0.8) ;
#3612 = CYLINDRICAL_SURFACE('',#4116,0.8) ;
#3613 = CYLINDRICAL_SURFACE('',#4118,0.8) ;
#3614 = CYLINDRICAL_SURFACE('',#4126,0.6) ;
#3615 = CYLINDRICAL_SURFACE('',#4129,0.6) ;
#3616 = CYLINDRICAL_SURFACE('',#4133,0.6) ;
#3617 = CYLINDRICAL_SURFACE('',#4136,0.6) ;
#3618 = CYLINDRICAL_SURFACE('',#4140,0.6) ;
#3619 = CYLINDRICAL_SURFACE('',#4143,0.6) ;
#3620 = CYLINDRICAL_SURFACE('',#4146,0.6) ;
#3621 = CYLINDRICAL_SURFACE('',#4149,0.6) ;
#3622 = CYLINDRICAL_SURFACE('',#4153,0.6) ;
#3623 = CYLINDRICAL_SURFACE('',#4157,0.6) ;
#3624 = CYLINDRICAL_SURFACE('',#4196,27.5) ;
#3625 = CYLINDRICAL_SURFACE('',#4233,1.) ;
#3626 = CYLINDRICAL_SURFACE('',#4235,1.) ;
#3627 = CYLINDRICAL_SURFACE('',#4239,1.) ;
#3628 = CYLINDRICAL_SURFACE('',#4242,1.) ;
#3629 = CYLINDRICAL_SURFACE('',#4251,0.63) ;
#3630 = CYLINDRICAL_SURFACE('',#4254,0.63) ;
#3631 = CYLINDRICAL_SURFACE('',#4269,3.25) ;
#3632 = CYLINDRICAL_SURFACE('',#4274,3.25) ;
#3633 = CYLINDRICAL_SURFACE('',#4280,3.25) ;
#3634 = CYLINDRICAL_SURFACE('',#4285,3.25) ;
#3635 = CYLINDRICAL_SURFACE('',#4292,6.) ;
#3636 = CYLINDRICAL_SURFACE('',#4295,3.2) ;
#3637 = CYLINDRICAL_SURFACE('',#4301,6.) ;
#3638 = CYLINDRICAL_SURFACE('',#4304,3.2) ;
#3639 = CYLINDRICAL_SURFACE('',#4310,6.) ;
#3640 = CYLINDRICAL_SURFACE('',#4313,3.2) ;
#3641 = CYLINDRICAL_SURFACE('',#4319,6.) ;
#3642 = CYLINDRICAL_SURFACE('',#4322,3.2) ;
#3643 = CYLINDRICAL_SURFACE('',#4345,5.) ;
#3644 = CYLINDRICAL_SURFACE('',#4349,3.) ;
#3645 = CYLINDRICAL_SURFACE('',#4370,5.) ;
#3646 = CYLINDRICAL_SURFACE('',#4374,3.) ;
#3647 = CYLINDRICAL_SURFACE('',#4395,5.) ;
#3648 = CYLINDRICAL_SURFACE('',#4399,3.) ;
#3649 = CYLINDRICAL_SURFACE('',#4420,5.) ;
#3650 = CYLINDRICAL_SURFACE('',#4424,3.) ;
#3651 = ADVANCED_FACE('',(#327),#3603,.F.) ;
#3652 = ADVANCED_FACE('',(#328),#267,.F.) ;
#3653 = ADVANCED_FACE('',(#329),#268,.F.) ;
#3654 = ADVANCED_FACE('',(#330),#3604,.F.) ;
#3655 = ADVANCED_FACE('',(#331),#269,.F.) ;
#3656 = ADVANCED_FACE('',(#332),#3605,.F.) ;
#3657 = ADVANCED_FACE('',(#333),#270,.F.) ;
#3658 = ADVANCED_FACE('',(#334),#3606,.F.) ;
#3659 = ADVANCED_FACE('',(#335),#271,.F.) ;
#3660 = ADVANCED_FACE('',(#336),#3607,.F.) ;
#3661 = ADVANCED_FACE('',(#337),#272,.F.) ;
#3662 = ADVANCED_FACE('',(#338),#135,.T.) ;
#3663 = ADVANCED_FACE('',(#339),#273,.F.) ;
#3664 = ADVANCED_FACE('',(#340),#136,.T.) ;
#3665 = ADVANCED_FACE('',(#341),#274,.T.) ;
#3666 = ADVANCED_FACE('',(#342),#137,.T.) ;
#3667 = ADVANCED_FACE('',(#343),#275,.T.) ;
#3668 = ADVANCED_FACE('',(#344),#138,.F.) ;
#3669 = ADVANCED_FACE('',(#345),#276,.T.) ;
#3670 = ADVANCED_FACE('',(#346),#139,.F.) ;
#3671 = ADVANCED_FACE('',(#347),#277,.T.) ;
#3672 = ADVANCED_FACE('',(#348),#140,.F.) ;
#3673 = ADVANCED_FACE('',(#349),#278,.F.) ;
#3674 = ADVANCED_FACE('',(#350),#141,.F.) ;
#3675 = ADVANCED_FACE('',(#351),#279,.F.) ;
#3676 = ADVANCED_FACE('',(#352),#142,.F.) ;
#3677 = ADVANCED_FACE('',(#353),#280,.T.) ;
#3678 = ADVANCED_FACE('',(#354),#143,.F.) ;
#3679 = ADVANCED_FACE('',(#355),#281,.T.) ;
#3680 = ADVANCED_FACE('',(#356),#144,.T.) ;
#3681 = ADVANCED_FACE('',(#357),#282,.F.) ;
#3682 = ADVANCED_FACE('',(#358),#145,.F.) ;
#3683 = ADVANCED_FACE('',(#359),#283,.F.) ;
#3684 = ADVANCED_FACE('',(#360),#146,.T.) ;
#3685 = ADVANCED_FACE('',(#361),#284,.T.) ;
#3686 = ADVANCED_FACE('',(#362),#147,.F.) ;
#3687 = ADVANCED_FACE('',(#363),#285,.T.) ;
#3688 = ADVANCED_FACE('',(#364),#148,.T.) ;
#3689 = ADVANCED_FACE('',(#365),#286,.T.) ;
#3690 = ADVANCED_FACE('',(#366),#149,.F.) ;
#3691 = ADVANCED_FACE('',(#367),#287,.T.) ;
#3692 = ADVANCED_FACE('',(#368),#150,.F.) ;
#3693 = ADVANCED_FACE('',(#369),#288,.F.) ;
#3694 = ADVANCED_FACE('',(#370),#151,.F.) ;
#3695 = ADVANCED_FACE('',(#371),#152,.T.) ;
#3696 = ADVANCED_FACE('',(#372),#153,.F.) ;
#3697 = ADVANCED_FACE('',(#373),#3608,.F.) ;
#3698 = ADVANCED_FACE('',(#374),#3609,.F.) ;
#3699 = ADVANCED_FACE('',(#375),#3610,.F.) ;
#3700 = ADVANCED_FACE('',(#376),#3611,.F.) ;
#3701 = ADVANCED_FACE('',(#377),#3612,.F.) ;
#3702 = ADVANCED_FACE('',(#378),#3613,.F.) ;
#3703 = ADVANCED_FACE('',(#379),#154,.F.) ;
#3704 = ADVANCED_FACE('',(#380),#155,.T.) ;
#3705 = ADVANCED_FACE('',(#381),#156,.T.) ;
#3706 = ADVANCED_FACE('',(#382),#157,.T.) ;
#3707 = ADVANCED_FACE('',(#383,#103,#104),#158,.T.) ;
#3708 = ADVANCED_FACE('',(#384,#105,#106),#159,.T.) ;
#3709 = ADVANCED_FACE('',(#385),#3614,.T.) ;
#3710 = ADVANCED_FACE('',(#386),#160,.T.) ;
#3711 = ADVANCED_FACE('',(#387),#3615,.T.) ;
#3712 = ADVANCED_FACE('',(#388),#161,.T.) ;
#3713 = ADVANCED_FACE('',(#389,#107,#108),#162,.T.) ;
#3714 = ADVANCED_FACE('',(#390),#3616,.T.) ;
#3715 = ADVANCED_FACE('',(#391),#163,.T.) ;
#3716 = ADVANCED_FACE('',(#392),#3617,.T.) ;
#3717 = ADVANCED_FACE('',(#393),#164,.F.) ;
#3718 = ADVANCED_FACE('',(#394),#165,.T.) ;
#3719 = ADVANCED_FACE('',(#395),#3618,.T.) ;
#3720 = ADVANCED_FACE('',(#396),#166,.F.) ;
#3721 = ADVANCED_FACE('',(#397),#3619,.T.) ;
#3722 = ADVANCED_FACE('',(#398,#109,#110),#167,.T.) ;
#3723 = ADVANCED_FACE('',(#399),#3620,.T.) ;
#3724 = ADVANCED_FACE('',(#400),#168,.F.) ;
#3725 = ADVANCED_FACE('',(#401),#3621,.T.) ;
#3726 = ADVANCED_FACE('',(#402),#169,.F.) ;
#3727 = ADVANCED_FACE('',(#403),#170,.F.) ;
#3728 = ADVANCED_FACE('',(#404),#3622,.T.) ;
#3729 = ADVANCED_FACE('',(#405),#171,.T.) ;
#3730 = ADVANCED_FACE('',(#406),#172,.T.) ;
#3731 = ADVANCED_FACE('',(#407),#3623,.T.) ;
#3732 = ADVANCED_FACE('',(#408),#289,.F.) ;
#3733 = ADVANCED_FACE('',(#409),#173,.F.) ;
#3734 = ADVANCED_FACE('',(#410),#290,.T.) ;
#3735 = ADVANCED_FACE('',(#411),#174,.F.) ;
#3736 = ADVANCED_FACE('',(#412),#291,.T.) ;
#3737 = ADVANCED_FACE('',(#413),#175,.T.) ;
#3738 = ADVANCED_FACE('',(#414),#292,.T.) ;
#3739 = ADVANCED_FACE('',(#415),#176,.T.) ;
#3740 = ADVANCED_FACE('',(#416),#293,.T.) ;
#3741 = ADVANCED_FACE('',(#417),#177,.T.) ;
#3742 = ADVANCED_FACE('',(#418),#294,.F.) ;
#3743 = ADVANCED_FACE('',(#419),#178,.T.) ;
#3744 = ADVANCED_FACE('',(#420),#295,.F.) ;
#3745 = ADVANCED_FACE('',(#421),#179,.T.) ;
#3746 = ADVANCED_FACE('',(#422),#296,.T.) ;
#3747 = ADVANCED_FACE('',(#423),#180,.T.) ;
#3748 = ADVANCED_FACE('',(#424),#297,.T.) ;
#3749 = ADVANCED_FACE('',(#425),#181,.F.) ;
#3750 = ADVANCED_FACE('',(#426),#298,.F.) ;
#3751 = ADVANCED_FACE('',(#427),#182,.T.) ;
#3752 = ADVANCED_FACE('',(#428),#299,.F.) ;
#3753 = ADVANCED_FACE('',(#429),#183,.F.) ;
#3754 = ADVANCED_FACE('',(#430),#300,.T.) ;
#3755 = ADVANCED_FACE('',(#431),#184,.T.) ;
#3756 = ADVANCED_FACE('',(#432),#301,.T.) ;
#3757 = ADVANCED_FACE('',(#433),#185,.F.) ;
#3758 = ADVANCED_FACE('',(#434),#302,.T.) ;
#3759 = ADVANCED_FACE('',(#435),#186,.T.) ;
#3760 = ADVANCED_FACE('',(#436),#303,.T.) ;
#3761 = ADVANCED_FACE('',(#437),#187,.T.) ;
#3762 = ADVANCED_FACE('',(#438),#304,.F.) ;
#3763 = ADVANCED_FACE('',(#439),#188,.T.) ;
#3764 = ADVANCED_FACE('',(#440),#189,.F.) ;
#3765 = ADVANCED_FACE('',(#441),#305,.F.) ;
#3766 = ADVANCED_FACE('',(#442),#3624,.F.) ;
#3767 = ADVANCED_FACE('',(#443),#306,.F.) ;
#3768 = ADVANCED_FACE('',(#444),#190,.T.) ;
#3769 = ADVANCED_FACE('',(#445),#307,.T.) ;
#3770 = ADVANCED_FACE('',(#446),#191,.F.) ;
#3771 = ADVANCED_FACE('',(#447),#308,.F.) ;
#3772 = ADVANCED_FACE('',(#448),#192,.F.) ;
#3773 = ADVANCED_FACE('',(#449),#309,.T.) ;
#3774 = ADVANCED_FACE('',(#450),#193,.F.) ;
#3775 = ADVANCED_FACE('',(#451),#310,.T.) ;
#3776 = ADVANCED_FACE('',(#452),#194,.T.) ;
#3777 = ADVANCED_FACE('',(#453),#311,.F.) ;
#3778 = ADVANCED_FACE('',(#454),#195,.F.) ;
#3779 = ADVANCED_FACE('',(#455),#312,.T.) ;
#3780 = ADVANCED_FACE('',(#456),#196,.T.) ;
#3781 = ADVANCED_FACE('',(#457),#197,.F.) ;
#3782 = ADVANCED_FACE('',(#458),#198,.F.) ;
#3783 = ADVANCED_FACE('',(#459),#3625,.F.) ;
#3784 = ADVANCED_FACE('',(#460),#3626,.T.) ;
#3785 = ADVANCED_FACE('',(#461),#199,.T.) ;
#3786 = ADVANCED_FACE('',(#462),#200,.F.) ;
#3787 = ADVANCED_FACE('',(#463),#3627,.T.) ;
#3788 = ADVANCED_FACE('',(#464),#201,.T.) ;
#3789 = ADVANCED_FACE('',(#465),#3628,.F.) ;
#3790 = ADVANCED_FACE('',(#466,#111,#112),#202,.T.) ;
#3791 = ADVANCED_FACE('',(#467,#113,#114),#203,.T.) ;
#3792 = ADVANCED_FACE('',(#468),#204,.F.) ;
#3793 = ADVANCED_FACE('',(#469),#3629,.T.) ;
#3794 = ADVANCED_FACE('',(#470),#205,.T.) ;
#3795 = ADVANCED_FACE('',(#471),#3630,.T.) ;
#3796 = ADVANCED_FACE('',(#472),#313,.T.) ;
#3797 = ADVANCED_FACE('',(#473),#206,.T.) ;
#3798 = ADVANCED_FACE('',(#474),#314,.F.) ;
#3799 = ADVANCED_FACE('',(#475),#207,.T.) ;
#3800 = ADVANCED_FACE('',(#476),#315,.T.) ;
#3801 = ADVANCED_FACE('',(#477),#208,.T.) ;
#3802 = ADVANCED_FACE('',(#478),#316,.T.) ;
#3803 = ADVANCED_FACE('',(#479),#209,.F.) ;
#3804 = ADVANCED_FACE('',(#480),#317,.F.) ;
#3805 = ADVANCED_FACE('',(#481),#210,.T.) ;
#3806 = ADVANCED_FACE('',(#482),#318,.T.) ;
#3807 = ADVANCED_FACE('',(#483),#211,.F.) ;
#3808 = ADVANCED_FACE('',(#484),#212,.T.) ;
#3809 = ADVANCED_FACE('',(#485),#3631,.F.) ;
#3810 = ADVANCED_FACE('',(#486),#319,.F.) ;
#3811 = ADVANCED_FACE('',(#487),#3632,.F.) ;
#3812 = ADVANCED_FACE('',(#488,#115,#116),#213,.T.) ;
#3813 = ADVANCED_FACE('',(#489),#320,.F.) ;
#3814 = ADVANCED_FACE('',(#490),#3633,.F.) ;
#3815 = ADVANCED_FACE('',(#491),#321,.F.) ;
#3816 = ADVANCED_FACE('',(#492),#3634,.F.) ;
#3817 = ADVANCED_FACE('',(#493,#117,#118),#214,.T.) ;
#3818 = ADVANCED_FACE('',(#494),#322,.F.) ;
#3819 = ADVANCED_FACE('',(#495),#3635,.T.) ;
#3820 = ADVANCED_FACE('',(#496),#3636,.F.) ;
#3821 = ADVANCED_FACE('',(#497,#119),#215,.F.) ;
#3822 = ADVANCED_FACE('',(#498,#120),#216,.T.) ;
#3823 = ADVANCED_FACE('',(#499),#3637,.T.) ;
#3824 = ADVANCED_FACE('',(#500),#3638,.F.) ;
#3825 = ADVANCED_FACE('',(#501,#121),#217,.F.) ;
#3826 = ADVANCED_FACE('',(#502,#122),#218,.T.) ;
#3827 = ADVANCED_FACE('',(#503),#3639,.T.) ;
#3828 = ADVANCED_FACE('',(#504),#3640,.F.) ;
#3829 = ADVANCED_FACE('',(#505,#123),#219,.F.) ;
#3830 = ADVANCED_FACE('',(#506,#124),#220,.T.) ;
#3831 = ADVANCED_FACE('',(#507),#3641,.T.) ;
#3832 = ADVANCED_FACE('',(#508),#3642,.F.) ;
#3833 = ADVANCED_FACE('',(#509,#125),#221,.F.) ;
#3834 = ADVANCED_FACE('',(#510,#126),#222,.T.) ;
#3835 = ADVANCED_FACE('',(#511),#223,.T.) ;
#3836 = ADVANCED_FACE('',(#512),#224,.T.) ;
#3837 = ADVANCED_FACE('',(#513),#225,.T.) ;
#3838 = ADVANCED_FACE('',(#514),#226,.T.) ;
#3839 = ADVANCED_FACE('',(#515),#227,.T.) ;
#3840 = ADVANCED_FACE('',(#516),#228,.T.) ;
#3841 = ADVANCED_FACE('',(#517),#229,.T.) ;
#3842 = ADVANCED_FACE('',(#518,#127),#230,.T.) ;
#3843 = ADVANCED_FACE('',(#519,#128),#231,.F.) ;
#3844 = ADVANCED_FACE('',(#520),#232,.F.) ;
#3845 = ADVANCED_FACE('',(#521),#51,.T.) ;
#3846 = ADVANCED_FACE('',(#522),#3643,.T.) ;
#3847 = ADVANCED_FACE('',(#523),#52,.F.) ;
#3848 = ADVANCED_FACE('',(#524),#3644,.T.) ;
#3849 = ADVANCED_FACE('',(#525),#323,.T.) ;
#3850 = ADVANCED_FACE('',(#526),#233,.T.) ;
#3851 = ADVANCED_FACE('',(#527),#234,.T.) ;
#3852 = ADVANCED_FACE('',(#528),#235,.T.) ;
#3853 = ADVANCED_FACE('',(#529),#236,.T.) ;
#3854 = ADVANCED_FACE('',(#530),#237,.T.) ;
#3855 = ADVANCED_FACE('',(#531),#238,.T.) ;
#3856 = ADVANCED_FACE('',(#532),#239,.T.) ;
#3857 = ADVANCED_FACE('',(#533,#129),#240,.T.) ;
#3858 = ADVANCED_FACE('',(#534,#130),#241,.F.) ;
#3859 = ADVANCED_FACE('',(#535),#242,.F.) ;
#3860 = ADVANCED_FACE('',(#536),#53,.T.) ;
#3861 = ADVANCED_FACE('',(#537),#3645,.T.) ;
#3862 = ADVANCED_FACE('',(#538),#54,.F.) ;
#3863 = ADVANCED_FACE('',(#539),#3646,.T.) ;
#3864 = ADVANCED_FACE('',(#540),#324,.T.) ;
#3865 = ADVANCED_FACE('',(#541),#243,.T.) ;
#3866 = ADVANCED_FACE('',(#542),#244,.T.) ;
#3867 = ADVANCED_FACE('',(#543),#245,.T.) ;
#3868 = ADVANCED_FACE('',(#544),#246,.T.) ;
#3869 = ADVANCED_FACE('',(#545),#247,.T.) ;
#3870 = ADVANCED_FACE('',(#546),#248,.T.) ;
#3871 = ADVANCED_FACE('',(#547),#249,.T.) ;
#3872 = ADVANCED_FACE('',(#548,#131),#250,.T.) ;
#3873 = ADVANCED_FACE('',(#549,#132),#251,.F.) ;
#3874 = ADVANCED_FACE('',(#550),#252,.F.) ;
#3875 = ADVANCED_FACE('',(#551),#55,.T.) ;
#3876 = ADVANCED_FACE('',(#552),#3647,.T.) ;
#3877 = ADVANCED_FACE('',(#553),#56,.F.) ;
#3878 = ADVANCED_FACE('',(#554),#3648,.T.) ;
#3879 = ADVANCED_FACE('',(#555),#325,.T.) ;
#3880 = ADVANCED_FACE('',(#556),#253,.T.) ;
#3881 = ADVANCED_FACE('',(#557),#254,.T.) ;
#3882 = ADVANCED_FACE('',(#558),#255,.T.) ;
#3883 = ADVANCED_FACE('',(#559),#256,.T.) ;
#3884 = ADVANCED_FACE('',(#560),#257,.T.) ;
#3885 = ADVANCED_FACE('',(#561),#258,.T.) ;
#3886 = ADVANCED_FACE('',(#562),#259,.T.) ;
#3887 = ADVANCED_FACE('',(#563,#133),#260,.T.) ;
#3888 = ADVANCED_FACE('',(#564,#134),#261,.F.) ;
#3889 = ADVANCED_FACE('',(#565),#262,.F.) ;
#3890 = ADVANCED_FACE('',(#566),#57,.T.) ;
#3891 = ADVANCED_FACE('',(#567),#3649,.T.) ;
#3892 = ADVANCED_FACE('',(#568),#58,.F.) ;
#3893 = ADVANCED_FACE('',(#569),#3650,.T.) ;
#3894 = ADVANCED_FACE('',(#570),#326,.T.) ;
#3895 = CLOSED_SHELL('',(#3651,#3652,#3653,#3654,#3655,#3656,#3657,#3658,
#3659,#3660,#3661,#3662,#3663,#3664,#3665,#3666,#3667,#3668,#3669,#3670,
#3671,#3672,#3673,#3674,#3675,#3676,#3677,#3678,#3679,#3680,#3681,#3682,
#3683,#3684,#3685,#3686,#3687,#3688,#3689,#3690,#3691,#3692,#3693,#3694,
#3695,#3696,#3697,#3698,#3699,#3700,#3701,#3702,#3703,#3704,#3705,#3706,
#3707,#3708,#3709,#3710,#3711,#3712,#3713,#3714,#3715,#3716,#3717,#3718,
#3719,#3720,#3721,#3722,#3723,#3724,#3725,#3726,#3727,#3728,#3729,#3730,
#3731,#3732,#3733,#3734,#3735,#3736,#3737,#3738,#3739,#3740,#3741,#3742,
#3743,#3744,#3745,#3746,#3747,#3748,#3749,#3750,#3751,#3752,#3753,#3754,
#3755,#3756,#3757,#3758,#3759,#3760,#3761,#3762,#3763,#3764)) ;
#3896 = CLOSED_SHELL('',(#3765,#3766,#3767,#3768,#3769,#3770,#3771,#3772,
#3773,#3774,#3775,#3776,#3777,#3778,#3779,#3780,#3781,#3782,#3783,#3784,
#3785,#3786,#3787,#3788,#3789,#3790,#3791,#3792,#3793,#3794,#3795,#3796,
#3797,#3798,#3799,#3800,#3801,#3802,#3803,#3804,#3805,#3806,#3807,#3808,
#3809,#3810,#3811,#3812,#3813,#3814,#3815,#3816,#3817,#3818)) ;
#3897 = CLOSED_SHELL('',(#3819,#3820,#3821,#3822)) ;
#3898 = CLOSED_SHELL('',(#3823,#3824,#3825,#3826)) ;
#3899 = CLOSED_SHELL('',(#3827,#3828,#3829,#3830)) ;
#3900 = CLOSED_SHELL('',(#3831,#3832,#3833,#3834)) ;
#3901 = CLOSED_SHELL('',(#3835,#3836,#3837,#3838,#3839,#3840,#3841,#3842,
#3843,#3844,#3845,#3846,#3847,#3848,#3849)) ;
#3902 = CLOSED_SHELL('',(#3850,#3851,#3852,#3853,#3854,#3855,#3856,#3857,
#3858,#3859,#3860,#3861,#3862,#3863,#3864)) ;
#3903 = CLOSED_SHELL('',(#3865,#3866,#3867,#3868,#3869,#3870,#3871,#3872,
#3873,#3874,#3875,#3876,#3877,#3878,#3879)) ;
#3904 = CLOSED_SHELL('',(#3880,#3881,#3882,#3883,#3884,#3885,#3886,#3887,
#3888,#3889,#3890,#3891,#3892,#3893,#3894)) ;
#3905 = DERIVED_UNIT_ELEMENT(#3925,1.) ;
#3906 = DERIVED_UNIT_ELEMENT(#6781,-3.) ;
#3907 = DERIVED_UNIT_ELEMENT(#3925,1.) ;
#3908 = DERIVED_UNIT_ELEMENT(#6781,-3.) ;
#3909 = DERIVED_UNIT_ELEMENT(#3925,1.) ;
#3910 = DERIVED_UNIT_ELEMENT(#6781,-3.) ;
#3911 = DERIVED_UNIT_ELEMENT(#3925,1.) ;
#3912 = DERIVED_UNIT_ELEMENT(#6781,-3.) ;
#3913 = DERIVED_UNIT_ELEMENT(#3925,1.) ;
#3914 = DERIVED_UNIT_ELEMENT(#6781,-3.) ;
#3915 = DERIVED_UNIT_ELEMENT(#3925,1.) ;
#3916 = DERIVED_UNIT_ELEMENT(#6781,-3.) ;
#3917 = DERIVED_UNIT_ELEMENT(#3925,1.) ;
#3918 = DERIVED_UNIT_ELEMENT(#6781,-3.) ;
#3919 = DERIVED_UNIT_ELEMENT(#3925,1.) ;
#3920 = DERIVED_UNIT_ELEMENT(#6781,-3.) ;
#3921 = DERIVED_UNIT_ELEMENT(#3925,1.) ;
#3922 = DERIVED_UNIT_ELEMENT(#6781,-3.) ;
#3923 = DERIVED_UNIT_ELEMENT(#3925,1.) ;
#3924 = DERIVED_UNIT_ELEMENT(#6781,-3.) ;
#3925 = (
MASS_UNIT()
NAMED_UNIT(*)
SI_UNIT(.KILO.,.GRAM.)
) ;
#3926 = DERIVED_UNIT((#3905,#3906)) ;
#3927 = DERIVED_UNIT((#3907,#3908)) ;
#3928 = DERIVED_UNIT((#3909,#3910)) ;
#3929 = DERIVED_UNIT((#3911,#3912)) ;
#3930 = DERIVED_UNIT((#3913,#3914)) ;
#3931 = DERIVED_UNIT((#3915,#3916)) ;
#3932 = DERIVED_UNIT((#3917,#3918)) ;
#3933 = DERIVED_UNIT((#3919,#3920)) ;
#3934 = DERIVED_UNIT((#3921,#3922)) ;
#3935 = DERIVED_UNIT((#3923,#3924)) ;
#3936 = MEASURE_REPRESENTATION_ITEM('density measure',
POSITIVE_RATIO_MEASURE(7850.),#3926) ;
#3937 = MEASURE_REPRESENTATION_ITEM('density measure',
POSITIVE_RATIO_MEASURE(7850.),#3927) ;
#3938 = MEASURE_REPRESENTATION_ITEM('density measure',
POSITIVE_RATIO_MEASURE(7850.),#3928) ;
#3939 = MEASURE_REPRESENTATION_ITEM('density measure',
POSITIVE_RATIO_MEASURE(7850.),#3929) ;
#3940 = MEASURE_REPRESENTATION_ITEM('density measure',
POSITIVE_RATIO_MEASURE(7850.),#3930) ;
#3941 = MEASURE_REPRESENTATION_ITEM('density measure',
POSITIVE_RATIO_MEASURE(7850.),#3931) ;
#3942 = MEASURE_REPRESENTATION_ITEM('density measure',
POSITIVE_RATIO_MEASURE(7850.),#3932) ;
#3943 = MEASURE_REPRESENTATION_ITEM('density measure',
POSITIVE_RATIO_MEASURE(7850.),#3933) ;
#3944 = MEASURE_REPRESENTATION_ITEM('density measure',
POSITIVE_RATIO_MEASURE(7850.),#3934) ;
#3945 = MEASURE_REPRESENTATION_ITEM('density measure',
POSITIVE_RATIO_MEASURE(7850.),#3935) ;
#3946 = PROPERTY_DEFINITION_REPRESENTATION(#3996,#3966) ;
#3947 = PROPERTY_DEFINITION_REPRESENTATION(#3997,#3967) ;
#3948 = PROPERTY_DEFINITION_REPRESENTATION(#3998,#3968) ;
#3949 = PROPERTY_DEFINITION_REPRESENTATION(#3999,#3969) ;
#3950 = PROPERTY_DEFINITION_REPRESENTATION(#4000,#3970) ;
#3951 = PROPERTY_DEFINITION_REPRESENTATION(#4001,#3971) ;
#3952 = PROPERTY_DEFINITION_REPRESENTATION(#4002,#3972) ;
#3953 = PROPERTY_DEFINITION_REPRESENTATION(#4003,#3973) ;
#3954 = PROPERTY_DEFINITION_REPRESENTATION(#4004,#3974) ;
#3955 = PROPERTY_DEFINITION_REPRESENTATION(#4005,#3975) ;
#3956 = PROPERTY_DEFINITION_REPRESENTATION(#4006,#3976) ;
#3957 = PROPERTY_DEFINITION_REPRESENTATION(#4007,#3977) ;
#3958 = PROPERTY_DEFINITION_REPRESENTATION(#4008,#3978) ;
#3959 = PROPERTY_DEFINITION_REPRESENTATION(#4009,#3979) ;
#3960 = PROPERTY_DEFINITION_REPRESENTATION(#4010,#3980) ;
#3961 = PROPERTY_DEFINITION_REPRESENTATION(#4011,#3981) ;
#3962 = PROPERTY_DEFINITION_REPRESENTATION(#4012,#3982) ;
#3963 = PROPERTY_DEFINITION_REPRESENTATION(#4013,#3983) ;
#3964 = PROPERTY_DEFINITION_REPRESENTATION(#4014,#3984) ;
#3965 = PROPERTY_DEFINITION_REPRESENTATION(#4015,#3985) ;
#3966 = REPRESENTATION('material name',(#3986),#6769) ;
#3967 = REPRESENTATION('density',(#3936),#6769) ;
#3968 = REPRESENTATION('material name',(#3987),#6770) ;
#3969 = REPRESENTATION('density',(#3937),#6770) ;
#3970 = REPRESENTATION('material name',(#3988),#6771) ;
#3971 = REPRESENTATION('density',(#3938),#6771) ;
#3972 = REPRESENTATION('material name',(#3989),#6772) ;
#3973 = REPRESENTATION('density',(#3939),#6772) ;
#3974 = REPRESENTATION('material name',(#3990),#6773) ;
#3975 = REPRESENTATION('density',(#3940),#6773) ;
#3976 = REPRESENTATION('material name',(#3991),#6774) ;
#3977 = REPRESENTATION('density',(#3941),#6774) ;
#3978 = REPRESENTATION('material name',(#3992),#6775) ;
#3979 = REPRESENTATION('density',(#3942),#6775) ;
#3980 = REPRESENTATION('material name',(#3993),#6776) ;
#3981 = REPRESENTATION('density',(#3943),#6776) ;
#3982 = REPRESENTATION('material name',(#3994),#6777) ;
#3983 = REPRESENTATION('density',(#3944),#6777) ;
#3984 = REPRESENTATION('material name',(#3995),#6778) ;
#3985 = REPRESENTATION('density',(#3945),#6778) ;
#3986 = DESCRIPTIVE_REPRESENTATION_ITEM('Steel','Steel') ;
#3987 = DESCRIPTIVE_REPRESENTATION_ITEM('Steel','Steel') ;
#3988 = DESCRIPTIVE_REPRESENTATION_ITEM('Steel','Steel') ;
#3989 = DESCRIPTIVE_REPRESENTATION_ITEM('Steel','Steel') ;
#3990 = DESCRIPTIVE_REPRESENTATION_ITEM('Steel','Steel') ;
#3991 = DESCRIPTIVE_REPRESENTATION_ITEM('Steel','Steel') ;
#3992 = DESCRIPTIVE_REPRESENTATION_ITEM('Steel','Steel') ;
#3993 = DESCRIPTIVE_REPRESENTATION_ITEM('Steel','Steel') ;
#3994 = DESCRIPTIVE_REPRESENTATION_ITEM('Steel','Steel') ;
#3995 = DESCRIPTIVE_REPRESENTATION_ITEM('Steel','Steel') ;
#3996 = PROPERTY_DEFINITION('material property','material name',#6829) ;
#3997 = PROPERTY_DEFINITION('material property','density of part',#6829) ;
#3998 = PROPERTY_DEFINITION('material property','material name',#6830) ;
#3999 = PROPERTY_DEFINITION('material property','density of part',#6830) ;
#4000 = PROPERTY_DEFINITION('material property','material name',#6831) ;
#4001 = PROPERTY_DEFINITION('material property','density of part',#6831) ;
#4002 = PROPERTY_DEFINITION('material property','material name',#6832) ;
#4003 = PROPERTY_DEFINITION('material property','density of part',#6832) ;
#4004 = PROPERTY_DEFINITION('material property','material name',#6833) ;
#4005 = PROPERTY_DEFINITION('material property','density of part',#6833) ;
#4006 = PROPERTY_DEFINITION('material property','material name',#6834) ;
#4007 = PROPERTY_DEFINITION('material property','density of part',#6834) ;
#4008 = PROPERTY_DEFINITION('material property','material name',#6835) ;
#4009 = PROPERTY_DEFINITION('material property','density of part',#6835) ;
#4010 = PROPERTY_DEFINITION('material property','material name',#6836) ;
#4011 = PROPERTY_DEFINITION('material property','density of part',#6836) ;
#4012 = PROPERTY_DEFINITION('material property','material name',#6837) ;
#4013 = PROPERTY_DEFINITION('material property','density of part',#6837) ;
#4014 = PROPERTY_DEFINITION('material property','material name',#6838) ;
#4015 = PROPERTY_DEFINITION('material property','density of part',#6838) ;
#4016 = AXIS2_PLACEMENT_3D('',#5639,#4437,#4438) ;
#4017 = AXIS2_PLACEMENT_3D('',#5640,#4439,#4440) ;
#4018 = AXIS2_PLACEMENT_3D('',#5641,#4441,#4442) ;
#4019 = AXIS2_PLACEMENT_3D('',#5644,#4443,#4444) ;
#4020 = AXIS2_PLACEMENT_3D('',#5648,#4446,#4447) ;
#4021 = AXIS2_PLACEMENT_3D('',#5650,#4449,#4450) ;
#4022 = AXIS2_PLACEMENT_3D('',#5659,#4451,#4452) ;
#4023 = AXIS2_PLACEMENT_3D('',#5660,#4453,#4454) ;
#4024 = AXIS2_PLACEMENT_3D('',#5663,#4455,#4456) ;
#4025 = AXIS2_PLACEMENT_3D('',#5670,#4457,#4458) ;
#4026 = AXIS2_PLACEMENT_3D('',#5672,#4459,#4460) ;
#4027 = AXIS2_PLACEMENT_3D('',#5675,#4462,#4463) ;
#4028 = AXIS2_PLACEMENT_3D('',#5676,#4464,#4465) ;
#4029 = AXIS2_PLACEMENT_3D('',#5679,#4467,#4468) ;
#4030 = AXIS2_PLACEMENT_3D('',#5680,#4469,#4470) ;
#4031 = AXIS2_PLACEMENT_3D('',#5682,#4471,#4472) ;
#4032 = AXIS2_PLACEMENT_3D('',#5685,#4474,#4475) ;
#4033 = AXIS2_PLACEMENT_3D('',#5686,#4476,#4477) ;
#4034 = AXIS2_PLACEMENT_3D('',#5689,#4479,#4480) ;
#4035 = AXIS2_PLACEMENT_3D('',#5690,#4481,#4482) ;
#4036 = AXIS2_PLACEMENT_3D('',#5692,#4483,#4484) ;
#4037 = AXIS2_PLACEMENT_3D('',#5695,#4486,#4487) ;
#4038 = AXIS2_PLACEMENT_3D('',#5696,#4488,#4489) ;
#4039 = AXIS2_PLACEMENT_3D('',#5699,#4491,#4492) ;
#4040 = AXIS2_PLACEMENT_3D('',#5700,#4493,#4494) ;
#4041 = AXIS2_PLACEMENT_3D('',#5702,#4495,#4496) ;
#4042 = AXIS2_PLACEMENT_3D('',#5705,#4498,#4499) ;
#4043 = AXIS2_PLACEMENT_3D('',#5706,#4500,#4501) ;
#4044 = AXIS2_PLACEMENT_3D('',#5709,#4503,#4504) ;
#4045 = AXIS2_PLACEMENT_3D('',#5710,#4505,#4506) ;
#4046 = AXIS2_PLACEMENT_3D('',#5718,#4510,#4511) ;
#4047 = AXIS2_PLACEMENT_3D('',#5730,#4517,#4518) ;
#4048 = AXIS2_PLACEMENT_3D('',#5734,#4520,#4521) ;
#4049 = AXIS2_PLACEMENT_3D('',#5742,#4525,#4526) ;
#4050 = AXIS2_PLACEMENT_3D('',#5746,#4528,#4529) ;
#4051 = AXIS2_PLACEMENT_3D('',#5758,#4535,#4536) ;
#4052 = AXIS2_PLACEMENT_3D('',#5760,#4538,#4539) ;
#4053 = AXIS2_PLACEMENT_3D('',#5764,#4541,#4542) ;
#4054 = AXIS2_PLACEMENT_3D('',#5766,#4544,#4545) ;
#4055 = AXIS2_PLACEMENT_3D('',#5770,#4548,#4549) ;
#4056 = AXIS2_PLACEMENT_3D('',#5772,#4550,#4551) ;
#4057 = AXIS2_PLACEMENT_3D('',#5774,#4553,#4554) ;
#4058 = AXIS2_PLACEMENT_3D('',#5778,#4557,#4558) ;
#4059 = AXIS2_PLACEMENT_3D('',#5780,#4559,#4560) ;
#4060 = AXIS2_PLACEMENT_3D('',#5782,#4562,#4563) ;
#4061 = AXIS2_PLACEMENT_3D('',#5786,#4566,#4567) ;
#4062 = AXIS2_PLACEMENT_3D('',#5788,#4568,#4569) ;
#4063 = AXIS2_PLACEMENT_3D('',#5790,#4571,#4572) ;
#4064 = AXIS2_PLACEMENT_3D('',#5794,#4575,#4576) ;
#4065 = AXIS2_PLACEMENT_3D('',#5796,#4577,#4578) ;
#4066 = AXIS2_PLACEMENT_3D('',#5798,#4580,#4581) ;
#4067 = AXIS2_PLACEMENT_3D('',#5802,#4584,#4585) ;
#4068 = AXIS2_PLACEMENT_3D('',#5804,#4586,#4587) ;
#4069 = AXIS2_PLACEMENT_3D('',#5806,#4589,#4590) ;
#4070 = AXIS2_PLACEMENT_3D('',#5810,#4593,#4594) ;
#4071 = AXIS2_PLACEMENT_3D('',#5812,#4595,#4596) ;
#4072 = AXIS2_PLACEMENT_3D('',#5814,#4598,#4599) ;
#4073 = AXIS2_PLACEMENT_3D('',#5818,#4602,#4603) ;
#4074 = AXIS2_PLACEMENT_3D('',#5820,#4604,#4605) ;
#4075 = AXIS2_PLACEMENT_3D('',#5822,#4607,#4608) ;
#4076 = AXIS2_PLACEMENT_3D('',#5826,#4611,#4612) ;
#4077 = AXIS2_PLACEMENT_3D('',#5828,#4613,#4614) ;
#4078 = AXIS2_PLACEMENT_3D('',#5830,#4616,#4617) ;
#4079 = AXIS2_PLACEMENT_3D('',#5834,#4620,#4621) ;
#4080 = AXIS2_PLACEMENT_3D('',#5836,#4622,#4623) ;
#4081 = AXIS2_PLACEMENT_3D('',#5838,#4625,#4626) ;
#4082 = AXIS2_PLACEMENT_3D('',#5842,#4629,#4630) ;
#4083 = AXIS2_PLACEMENT_3D('',#5844,#4631,#4632) ;
#4084 = AXIS2_PLACEMENT_3D('',#5846,#4634,#4635) ;
#4085 = AXIS2_PLACEMENT_3D('',#5850,#4638,#4639) ;
#4086 = AXIS2_PLACEMENT_3D('',#5852,#4640,#4641) ;
#4087 = AXIS2_PLACEMENT_3D('',#5854,#4643,#4644) ;
#4088 = AXIS2_PLACEMENT_3D('',#5858,#4647,#4648) ;
#4089 = AXIS2_PLACEMENT_3D('',#5860,#4649,#4650) ;
#4090 = AXIS2_PLACEMENT_3D('',#5862,#4652,#4653) ;
#4091 = AXIS2_PLACEMENT_3D('',#5866,#4656,#4657) ;
#4092 = AXIS2_PLACEMENT_3D('',#5868,#4658,#4659) ;
#4093 = AXIS2_PLACEMENT_3D('',#5870,#4661,#4662) ;
#4094 = AXIS2_PLACEMENT_3D('',#5874,#4665,#4666) ;
#4095 = AXIS2_PLACEMENT_3D('',#5876,#4667,#4668) ;
#4096 = AXIS2_PLACEMENT_3D('',#5878,#4670,#4671) ;
#4097 = AXIS2_PLACEMENT_3D('',#5882,#4674,#4675) ;
#4098 = AXIS2_PLACEMENT_3D('',#5884,#4676,#4677) ;
#4099 = AXIS2_PLACEMENT_3D('',#5886,#4679,#4680) ;
#4100 = AXIS2_PLACEMENT_3D('',#5890,#4683,#4684) ;
#4101 = AXIS2_PLACEMENT_3D('',#5894,#4687,#4688) ;
#4102 = AXIS2_PLACEMENT_3D('',#5899,#4690,#4691) ;
#4103 = AXIS2_PLACEMENT_3D('',#5911,#4697,#4698) ;
#4104 = AXIS2_PLACEMENT_3D('',#5915,#4700,#4701) ;
#4105 = AXIS2_PLACEMENT_3D('',#5923,#4705,#4706) ;
#4106 = AXIS2_PLACEMENT_3D('',#5927,#4708,#4709) ;
#4107 = AXIS2_PLACEMENT_3D('',#5939,#4715,#4716) ;
#4108 = AXIS2_PLACEMENT_3D('',#5944,#4720,#4721) ;
#4109 = AXIS2_PLACEMENT_3D('',#5947,#4722,#4723) ;
#4110 = AXIS2_PLACEMENT_3D('',#5950,#4726,#4727) ;
#4111 = AXIS2_PLACEMENT_3D('',#5953,#4728,#4729) ;
#4112 = AXIS2_PLACEMENT_3D('',#5956,#4732,#4733) ;
#4113 = AXIS2_PLACEMENT_3D('',#5959,#4734,#4735) ;
#4114 = AXIS2_PLACEMENT_3D('',#5962,#4738,#4739) ;
#4115 = AXIS2_PLACEMENT_3D('',#5965,#4740,#4741) ;
#4116 = AXIS2_PLACEMENT_3D('',#5968,#4744,#4745) ;
#4117 = AXIS2_PLACEMENT_3D('',#5971,#4746,#4747) ;
#4118 = AXIS2_PLACEMENT_3D('',#5974,#4750,#4751) ;
#4119 = AXIS2_PLACEMENT_3D('',#5977,#4752,#4753) ;
#4120 = AXIS2_PLACEMENT_3D('',#5980,#4756,#4757) ;
#4121 = AXIS2_PLACEMENT_3D('',#5984,#4760,#4761) ;
#4122 = AXIS2_PLACEMENT_3D('',#5986,#4763,#4764) ;
#4123 = AXIS2_PLACEMENT_3D('',#5988,#4766,#4767) ;
#4124 = AXIS2_PLACEMENT_3D('',#5992,#4770,#4771) ;
#4125 = AXIS2_PLACEMENT_3D('',#5994,#4773,#4774) ;
#4126 = AXIS2_PLACEMENT_3D('',#5996,#4776,#4777) ;
#4127 = AXIS2_PLACEMENT_3D('',#6001,#4780,#4781) ;
#4128 = AXIS2_PLACEMENT_3D('',#6002,#4782,#4783) ;
#4129 = AXIS2_PLACEMENT_3D('',#6006,#4786,#4787) ;
#4130 = AXIS2_PLACEMENT_3D('',#6009,#4789,#4790) ;
#4131 = AXIS2_PLACEMENT_3D('',#6010,#4791,#4792) ;
#4132 = AXIS2_PLACEMENT_3D('',#6014,#4795,#4796) ;
#4133 = AXIS2_PLACEMENT_3D('',#6018,#4799,#4800) ;
#4134 = AXIS2_PLACEMENT_3D('',#6019,#4801,#4802) ;
#4135 = AXIS2_PLACEMENT_3D('',#6020,#4803,#4804) ;
#4136 = AXIS2_PLACEMENT_3D('',#6024,#4807,#4808) ;
#4137 = AXIS2_PLACEMENT_3D('',#6027,#4810,#4811) ;
#4138 = AXIS2_PLACEMENT_3D('',#6028,#4812,#4813) ;
#4139 = AXIS2_PLACEMENT_3D('',#6032,#4816,#4817) ;
#4140 = AXIS2_PLACEMENT_3D('',#6036,#4820,#4821) ;
#4141 = AXIS2_PLACEMENT_3D('',#6037,#4822,#4823) ;
#4142 = AXIS2_PLACEMENT_3D('',#6038,#4824,#4825) ;
#4143 = AXIS2_PLACEMENT_3D('',#6042,#4828,#4829) ;
#4144 = AXIS2_PLACEMENT_3D('',#6045,#4831,#4832) ;
#4145 = AXIS2_PLACEMENT_3D('',#6046,#4833,#4834) ;
#4146 = AXIS2_PLACEMENT_3D('',#6050,#4837,#4838) ;
#4147 = AXIS2_PLACEMENT_3D('',#6053,#4840,#4841) ;
#4148 = AXIS2_PLACEMENT_3D('',#6054,#4842,#4843) ;
#4149 = AXIS2_PLACEMENT_3D('',#6058,#4846,#4847) ;
#4150 = AXIS2_PLACEMENT_3D('',#6061,#4849,#4850) ;
#4151 = AXIS2_PLACEMENT_3D('',#6062,#4851,#4852) ;
#4152 = AXIS2_PLACEMENT_3D('',#6066,#4855,#4856) ;
#4153 = AXIS2_PLACEMENT_3D('',#6070,#4859,#4860) ;
#4154 = AXIS2_PLACEMENT_3D('',#6071,#4861,#4862) ;
#4155 = AXIS2_PLACEMENT_3D('',#6072,#4863,#4864) ;
#4156 = AXIS2_PLACEMENT_3D('',#6076,#4867,#4868) ;
#4157 = AXIS2_PLACEMENT_3D('',#6080,#4871,#4872) ;
#4158 = AXIS2_PLACEMENT_3D('',#6081,#4873,#4874) ;
#4159 = AXIS2_PLACEMENT_3D('',#6082,#4875,#4876) ;
#4160 = AXIS2_PLACEMENT_3D('',#6085,#4879,#4880) ;
#4161 = AXIS2_PLACEMENT_3D('',#6087,#4882,#4883) ;
#4162 = AXIS2_PLACEMENT_3D('',#6089,#4885,#4886) ;
#4163 = AXIS2_PLACEMENT_3D('',#6091,#4888,#4889) ;
#4164 = AXIS2_PLACEMENT_3D('',#6093,#4891,#4892) ;
#4165 = AXIS2_PLACEMENT_3D('',#6095,#4894,#4895) ;
#4166 = AXIS2_PLACEMENT_3D('',#6097,#4897,#4898) ;
#4167 = AXIS2_PLACEMENT_3D('',#6099,#4900,#4901) ;
#4168 = AXIS2_PLACEMENT_3D('',#6101,#4903,#4904) ;
#4169 = AXIS2_PLACEMENT_3D('',#6103,#4906,#4907) ;
#4170 = AXIS2_PLACEMENT_3D('',#6105,#4909,#4910) ;
#4171 = AXIS2_PLACEMENT_3D('',#6107,#4912,#4913) ;
#4172 = AXIS2_PLACEMENT_3D('',#6109,#4915,#4916) ;
#4173 = AXIS2_PLACEMENT_3D('',#6111,#4918,#4919) ;
#4174 = AXIS2_PLACEMENT_3D('',#6113,#4921,#4922) ;
#4175 = AXIS2_PLACEMENT_3D('',#6115,#4924,#4925) ;
#4176 = AXIS2_PLACEMENT_3D('',#6117,#4927,#4928) ;
#4177 = AXIS2_PLACEMENT_3D('',#6119,#4930,#4931) ;
#4178 = AXIS2_PLACEMENT_3D('',#6121,#4933,#4934) ;
#4179 = AXIS2_PLACEMENT_3D('',#6123,#4936,#4937) ;
#4180 = AXIS2_PLACEMENT_3D('',#6125,#4939,#4940) ;
#4181 = AXIS2_PLACEMENT_3D('',#6127,#4942,#4943) ;
#4182 = AXIS2_PLACEMENT_3D('',#6129,#4945,#4946) ;
#4183 = AXIS2_PLACEMENT_3D('',#6131,#4948,#4949) ;
#4184 = AXIS2_PLACEMENT_3D('',#6133,#4951,#4952) ;
#4185 = AXIS2_PLACEMENT_3D('',#6135,#4954,#4955) ;
#4186 = AXIS2_PLACEMENT_3D('',#6137,#4957,#4958) ;
#4187 = AXIS2_PLACEMENT_3D('',#6139,#4960,#4961) ;
#4188 = AXIS2_PLACEMENT_3D('',#6141,#4963,#4964) ;
#4189 = AXIS2_PLACEMENT_3D('',#6143,#4966,#4967) ;
#4190 = AXIS2_PLACEMENT_3D('',#6145,#4969,#4970) ;
#4191 = AXIS2_PLACEMENT_3D('',#6146,#4971,#4972) ;
#4192 = AXIS2_PLACEMENT_3D('',#6147,#4973,#4974) ;
#4193 = AXIS2_PLACEMENT_3D('',#6148,#4975,#4976) ;
#4194 = AXIS2_PLACEMENT_3D('',#6156,#4977,#4978) ;
#4195 = AXIS2_PLACEMENT_3D('',#6162,#4979,#4980) ;
#4196 = AXIS2_PLACEMENT_3D('',#6163,#4981,#4982) ;
#4197 = AXIS2_PLACEMENT_3D('',#6167,#4984,#4985) ;
#4198 = AXIS2_PLACEMENT_3D('',#6169,#4987,#4988) ;
#4199 = AXIS2_PLACEMENT_3D('',#6172,#4989,#4990) ;
#4200 = AXIS2_PLACEMENT_3D('',#6181,#4991,#4992) ;
#4201 = AXIS2_PLACEMENT_3D('',#6189,#4996,#4997) ;
#4202 = AXIS2_PLACEMENT_3D('',#6193,#4999,#5000) ;
#4203 = AXIS2_PLACEMENT_3D('',#6197,#5002,#5003) ;
#4204 = AXIS2_PLACEMENT_3D('',#6201,#5005,#5006) ;
#4205 = AXIS2_PLACEMENT_3D('',#6205,#5008,#5009) ;
#4206 = AXIS2_PLACEMENT_3D('',#6209,#5011,#5012) ;
#4207 = AXIS2_PLACEMENT_3D('',#6211,#5014,#5015) ;
#4208 = AXIS2_PLACEMENT_3D('',#6215,#5017,#5018) ;
#4209 = AXIS2_PLACEMENT_3D('',#6217,#5020,#5021) ;
#4210 = AXIS2_PLACEMENT_3D('',#6221,#5024,#5025) ;
#4211 = AXIS2_PLACEMENT_3D('',#6223,#5026,#5027) ;
#4212 = AXIS2_PLACEMENT_3D('',#6225,#5029,#5030) ;
#4213 = AXIS2_PLACEMENT_3D('',#6229,#5033,#5034) ;
#4214 = AXIS2_PLACEMENT_3D('',#6231,#5035,#5036) ;
#4215 = AXIS2_PLACEMENT_3D('',#6233,#5038,#5039) ;
#4216 = AXIS2_PLACEMENT_3D('',#6237,#5042,#5043) ;
#4217 = AXIS2_PLACEMENT_3D('',#6239,#5044,#5045) ;
#4218 = AXIS2_PLACEMENT_3D('',#6241,#5047,#5048) ;
#4219 = AXIS2_PLACEMENT_3D('',#6245,#5051,#5052) ;
#4220 = AXIS2_PLACEMENT_3D('',#6247,#5053,#5054) ;
#4221 = AXIS2_PLACEMENT_3D('',#6249,#5056,#5057) ;
#4222 = AXIS2_PLACEMENT_3D('',#6253,#5060,#5061) ;
#4223 = AXIS2_PLACEMENT_3D('',#6255,#5062,#5063) ;
#4224 = AXIS2_PLACEMENT_3D('',#6257,#5065,#5066) ;
#4225 = AXIS2_PLACEMENT_3D('',#6261,#5069,#5070) ;
#4226 = AXIS2_PLACEMENT_3D('',#6265,#5073,#5074) ;
#4227 = AXIS2_PLACEMENT_3D('',#6270,#5076,#5077) ;
#4228 = AXIS2_PLACEMENT_3D('',#6274,#5079,#5080) ;
#4229 = AXIS2_PLACEMENT_3D('',#6278,#5082,#5083) ;
#4230 = AXIS2_PLACEMENT_3D('',#6282,#5085,#5086) ;
#4231 = AXIS2_PLACEMENT_3D('',#6286,#5088,#5089) ;
#4232 = AXIS2_PLACEMENT_3D('',#6290,#5091,#5092) ;
#4233 = AXIS2_PLACEMENT_3D('',#6295,#5096,#5097) ;
#4234 = AXIS2_PLACEMENT_3D('',#6298,#5098,#5099) ;
#4235 = AXIS2_PLACEMENT_3D('',#6301,#5102,#5103) ;
#4236 = AXIS2_PLACEMENT_3D('',#6306,#5106,#5107) ;
#4237 = AXIS2_PLACEMENT_3D('',#6307,#5108,#5109) ;
#4238 = AXIS2_PLACEMENT_3D('',#6311,#5112,#5113) ;
#4239 = AXIS2_PLACEMENT_3D('',#6315,#5116,#5117) ;
#4240 = AXIS2_PLACEMENT_3D('',#6318,#5119,#5120) ;
#4241 = AXIS2_PLACEMENT_3D('',#6319,#5121,#5122) ;
#4242 = AXIS2_PLACEMENT_3D('',#6321,#5124,#5125) ;
#4243 = AXIS2_PLACEMENT_3D('',#6323,#5126,#5127) ;
#4244 = AXIS2_PLACEMENT_3D('',#6325,#5129,#5130) ;
#4245 = AXIS2_PLACEMENT_3D('',#6330,#5133,#5134) ;
#4246 = AXIS2_PLACEMENT_3D('',#6332,#5135,#5136) ;
#4247 = AXIS2_PLACEMENT_3D('',#6333,#5137,#5138) ;
#4248 = AXIS2_PLACEMENT_3D('',#6338,#5141,#5142) ;
#4249 = AXIS2_PLACEMENT_3D('',#6340,#5143,#5144) ;
#4250 = AXIS2_PLACEMENT_3D('',#6341,#5145,#5146) ;
#4251 = AXIS2_PLACEMENT_3D('',#6345,#5149,#5150) ;
#4252 = AXIS2_PLACEMENT_3D('',#6348,#5152,#5153) ;
#4253 = AXIS2_PLACEMENT_3D('',#6349,#5154,#5155) ;
#4254 = AXIS2_PLACEMENT_3D('',#6353,#5158,#5159) ;
#4255 = AXIS2_PLACEMENT_3D('',#6356,#5161,#5162) ;
#4256 = AXIS2_PLACEMENT_3D('',#6357,#5163,#5164) ;
#4257 = AXIS2_PLACEMENT_3D('',#6360,#5167,#5168) ;
#4258 = AXIS2_PLACEMENT_3D('',#6363,#5171,#5172) ;
#4259 = AXIS2_PLACEMENT_3D('',#6365,#5174,#5175) ;
#4260 = AXIS2_PLACEMENT_3D('',#6367,#5177,#5178) ;
#4261 = AXIS2_PLACEMENT_3D('',#6369,#5180,#5181) ;
#4262 = AXIS2_PLACEMENT_3D('',#6371,#5183,#5184) ;
#4263 = AXIS2_PLACEMENT_3D('',#6373,#5186,#5187) ;
#4264 = AXIS2_PLACEMENT_3D('',#6375,#5189,#5190) ;
#4265 = AXIS2_PLACEMENT_3D('',#6377,#5192,#5193) ;
#4266 = AXIS2_PLACEMENT_3D('',#6380,#5196,#5197) ;
#4267 = AXIS2_PLACEMENT_3D('',#6382,#5199,#5200) ;
#4268 = AXIS2_PLACEMENT_3D('',#6383,#5201,#5202) ;
#4269 = AXIS2_PLACEMENT_3D('',#6384,#5203,#5204) ;
#4270 = AXIS2_PLACEMENT_3D('',#6387,#5205,#5206) ;
#4271 = AXIS2_PLACEMENT_3D('',#6389,#5208,#5209) ;
#4272 = AXIS2_PLACEMENT_3D('',#6390,#5210,#5211) ;
#4273 = AXIS2_PLACEMENT_3D('',#6393,#5213,#5214) ;
#4274 = AXIS2_PLACEMENT_3D('',#6394,#5215,#5216) ;
#4275 = AXIS2_PLACEMENT_3D('',#6397,#5217,#5218) ;
#4276 = AXIS2_PLACEMENT_3D('',#6399,#5220,#5221) ;
#4277 = AXIS2_PLACEMENT_3D('',#6400,#5222,#5223) ;
#4278 = AXIS2_PLACEMENT_3D('',#6402,#5224,#5225) ;
#4279 = AXIS2_PLACEMENT_3D('',#6403,#5226,#5227) ;
#4280 = AXIS2_PLACEMENT_3D('',#6405,#5229,#5230) ;
#4281 = AXIS2_PLACEMENT_3D('',#6408,#5231,#5232) ;
#4282 = AXIS2_PLACEMENT_3D('',#6410,#5234,#5235) ;
#4283 = AXIS2_PLACEMENT_3D('',#6411,#5236,#5237) ;
#4284 = AXIS2_PLACEMENT_3D('',#6414,#5239,#5240) ;
#4285 = AXIS2_PLACEMENT_3D('',#6415,#5241,#5242) ;
#4286 = AXIS2_PLACEMENT_3D('',#6418,#5243,#5244) ;
#4287 = AXIS2_PLACEMENT_3D('',#6420,#5246,#5247) ;
#4288 = AXIS2_PLACEMENT_3D('',#6421,#5248,#5249) ;
#4289 = AXIS2_PLACEMENT_3D('',#6423,#5250,#5251) ;
#4290 = AXIS2_PLACEMENT_3D('',#6424,#5252,#5253) ;
#4291 = AXIS2_PLACEMENT_3D('',#6426,#5255,#5256) ;
#4292 = AXIS2_PLACEMENT_3D('',#6427,#5257,#5258) ;
#4293 = AXIS2_PLACEMENT_3D('',#6429,#5259,#5260) ;
#4294 = AXIS2_PLACEMENT_3D('',#6432,#5262,#5263) ;
#4295 = AXIS2_PLACEMENT_3D('',#6433,#5264,#5265) ;
#4296 = AXIS2_PLACEMENT_3D('',#6435,#5266,#5267) ;
#4297 = AXIS2_PLACEMENT_3D('',#6438,#5269,#5270) ;
#4298 = AXIS2_PLACEMENT_3D('',#6439,#5271,#5272) ;
#4299 = AXIS2_PLACEMENT_3D('',#6440,#5273,#5274) ;
#4300 = AXIS2_PLACEMENT_3D('',#6441,#5275,#5276) ;
#4301 = AXIS2_PLACEMENT_3D('',#6442,#5277,#5278) ;
#4302 = AXIS2_PLACEMENT_3D('',#6444,#5279,#5280) ;
#4303 = AXIS2_PLACEMENT_3D('',#6447,#5282,#5283) ;
#4304 = AXIS2_PLACEMENT_3D('',#6448,#5284,#5285) ;
#4305 = AXIS2_PLACEMENT_3D('',#6450,#5286,#5287) ;
#4306 = AXIS2_PLACEMENT_3D('',#6453,#5289,#5290) ;
#4307 = AXIS2_PLACEMENT_3D('',#6454,#5291,#5292) ;
#4308 = AXIS2_PLACEMENT_3D('',#6455,#5293,#5294) ;
#4309 = AXIS2_PLACEMENT_3D('',#6456,#5295,#5296) ;
#4310 = AXIS2_PLACEMENT_3D('',#6457,#5297,#5298) ;
#4311 = AXIS2_PLACEMENT_3D('',#6459,#5299,#5300) ;
#4312 = AXIS2_PLACEMENT_3D('',#6462,#5302,#5303) ;
#4313 = AXIS2_PLACEMENT_3D('',#6463,#5304,#5305) ;
#4314 = AXIS2_PLACEMENT_3D('',#6465,#5306,#5307) ;
#4315 = AXIS2_PLACEMENT_3D('',#6468,#5309,#5310) ;
#4316 = AXIS2_PLACEMENT_3D('',#6469,#5311,#5312) ;
#4317 = AXIS2_PLACEMENT_3D('',#6470,#5313,#5314) ;
#4318 = AXIS2_PLACEMENT_3D('',#6471,#5315,#5316) ;
#4319 = AXIS2_PLACEMENT_3D('',#6472,#5317,#5318) ;
#4320 = AXIS2_PLACEMENT_3D('',#6474,#5319,#5320) ;
#4321 = AXIS2_PLACEMENT_3D('',#6477,#5322,#5323) ;
#4322 = AXIS2_PLACEMENT_3D('',#6478,#5324,#5325) ;
#4323 = AXIS2_PLACEMENT_3D('',#6480,#5326,#5327) ;
#4324 = AXIS2_PLACEMENT_3D('',#6483,#5329,#5330) ;
#4325 = AXIS2_PLACEMENT_3D('',#6484,#5331,#5332) ;
#4326 = AXIS2_PLACEMENT_3D('',#6485,#5333,#5334) ;
#4327 = AXIS2_PLACEMENT_3D('',#6486,#5335,#5336) ;
#4328 = AXIS2_PLACEMENT_3D('',#6487,#5337,#5338) ;
#4329 = AXIS2_PLACEMENT_3D('',#6496,#5343,#5344) ;
#4330 = AXIS2_PLACEMENT_3D('',#6502,#5348,#5349) ;
#4331 = AXIS2_PLACEMENT_3D('',#6508,#5353,#5354) ;
#4332 = AXIS2_PLACEMENT_3D('',#6514,#5358,#5359) ;
#4333 = AXIS2_PLACEMENT_3D('',#6518,#5362,#5363) ;
#4334 = AXIS2_PLACEMENT_3D('',#6522,#5366,#5367) ;
#4335 = AXIS2_PLACEMENT_3D('',#6524,#5369,#5370) ;
#4336 = AXIS2_PLACEMENT_3D('',#6526,#5371,#5372) ;
#4337 = AXIS2_PLACEMENT_3D('',#6527,#5373,#5374) ;
#4338 = AXIS2_PLACEMENT_3D('',#6529,#5375,#5376) ;
#4339 = AXIS2_PLACEMENT_3D('',#6531,#5377,#5378) ;
#4340 = AXIS2_PLACEMENT_3D('',#6532,#5379,#5380) ;
#4341 = AXIS2_PLACEMENT_3D('',#6534,#5381,#5382) ;
#4342 = AXIS2_PLACEMENT_3D('',#6535,#5383,#5384) ;
#4343 = AXIS2_PLACEMENT_3D('',#6537,#5385,#5386) ;
#4344 = AXIS2_PLACEMENT_3D('',#6538,#5387,#5388) ;
#4345 = AXIS2_PLACEMENT_3D('',#6539,#5389,#5390) ;
#4346 = AXIS2_PLACEMENT_3D('',#6541,#5392,#5393) ;
#4347 = AXIS2_PLACEMENT_3D('',#6543,#5394,#5395) ;
#4348 = AXIS2_PLACEMENT_3D('',#6544,#5396,#5397) ;
#4349 = AXIS2_PLACEMENT_3D('',#6545,#5398,#5399) ;
#4350 = AXIS2_PLACEMENT_3D('',#6548,#5401,#5402) ;
#4351 = AXIS2_PLACEMENT_3D('',#6549,#5403,#5404) ;
#4352 = AXIS2_PLACEMENT_3D('',#6551,#5406,#5407) ;
#4353 = AXIS2_PLACEMENT_3D('',#6552,#5408,#5409) ;
#4354 = AXIS2_PLACEMENT_3D('',#6561,#5414,#5415) ;
#4355 = AXIS2_PLACEMENT_3D('',#6567,#5419,#5420) ;
#4356 = AXIS2_PLACEMENT_3D('',#6573,#5424,#5425) ;
#4357 = AXIS2_PLACEMENT_3D('',#6579,#5429,#5430) ;
#4358 = AXIS2_PLACEMENT_3D('',#6583,#5433,#5434) ;
#4359 = AXIS2_PLACEMENT_3D('',#6587,#5437,#5438) ;
#4360 = AXIS2_PLACEMENT_3D('',#6589,#5440,#5441) ;
#4361 = AXIS2_PLACEMENT_3D('',#6591,#5442,#5443) ;
#4362 = AXIS2_PLACEMENT_3D('',#6592,#5444,#5445) ;
#4363 = AXIS2_PLACEMENT_3D('',#6594,#5446,#5447) ;
#4364 = AXIS2_PLACEMENT_3D('',#6596,#5448,#5449) ;
#4365 = AXIS2_PLACEMENT_3D('',#6597,#5450,#5451) ;
#4366 = AXIS2_PLACEMENT_3D('',#6599,#5452,#5453) ;
#4367 = AXIS2_PLACEMENT_3D('',#6600,#5454,#5455) ;
#4368 = AXIS2_PLACEMENT_3D('',#6602,#5456,#5457) ;
#4369 = AXIS2_PLACEMENT_3D('',#6603,#5458,#5459) ;
#4370 = AXIS2_PLACEMENT_3D('',#6604,#5460,#5461) ;
#4371 = AXIS2_PLACEMENT_3D('',#6606,#5463,#5464) ;
#4372 = AXIS2_PLACEMENT_3D('',#6608,#5465,#5466) ;
#4373 = AXIS2_PLACEMENT_3D('',#6609,#5467,#5468) ;
#4374 = AXIS2_PLACEMENT_3D('',#6610,#5469,#5470) ;
#4375 = AXIS2_PLACEMENT_3D('',#6613,#5472,#5473) ;
#4376 = AXIS2_PLACEMENT_3D('',#6614,#5474,#5475) ;
#4377 = AXIS2_PLACEMENT_3D('',#6616,#5477,#5478) ;
#4378 = AXIS2_PLACEMENT_3D('',#6617,#5479,#5480) ;
#4379 = AXIS2_PLACEMENT_3D('',#6626,#5485,#5486) ;
#4380 = AXIS2_PLACEMENT_3D('',#6632,#5490,#5491) ;
#4381 = AXIS2_PLACEMENT_3D('',#6638,#5495,#5496) ;
#4382 = AXIS2_PLACEMENT_3D('',#6644,#5500,#5501) ;
#4383 = AXIS2_PLACEMENT_3D('',#6648,#5504,#5505) ;
#4384 = AXIS2_PLACEMENT_3D('',#6652,#5508,#5509) ;
#4385 = AXIS2_PLACEMENT_3D('',#6654,#5511,#5512) ;
#4386 = AXIS2_PLACEMENT_3D('',#6656,#5513,#5514) ;
#4387 = AXIS2_PLACEMENT_3D('',#6657,#5515,#5516) ;
#4388 = AXIS2_PLACEMENT_3D('',#6659,#5517,#5518) ;
#4389 = AXIS2_PLACEMENT_3D('',#6661,#5519,#5520) ;
#4390 = AXIS2_PLACEMENT_3D('',#6662,#5521,#5522) ;
#4391 = AXIS2_PLACEMENT_3D('',#6664,#5523,#5524) ;
#4392 = AXIS2_PLACEMENT_3D('',#6665,#5525,#5526) ;
#4393 = AXIS2_PLACEMENT_3D('',#6667,#5527,#5528) ;
#4394 = AXIS2_PLACEMENT_3D('',#6668,#5529,#5530) ;
#4395 = AXIS2_PLACEMENT_3D('',#6669,#5531,#5532) ;
#4396 = AXIS2_PLACEMENT_3D('',#6671,#5534,#5535) ;
#4397 = AXIS2_PLACEMENT_3D('',#6673,#5536,#5537) ;
#4398 = AXIS2_PLACEMENT_3D('',#6674,#5538,#5539) ;
#4399 = AXIS2_PLACEMENT_3D('',#6675,#5540,#5541) ;
#4400 = AXIS2_PLACEMENT_3D('',#6678,#5543,#5544) ;
#4401 = AXIS2_PLACEMENT_3D('',#6679,#5545,#5546) ;
#4402 = AXIS2_PLACEMENT_3D('',#6681,#5548,#5549) ;
#4403 = AXIS2_PLACEMENT_3D('',#6682,#5550,#5551) ;
#4404 = AXIS2_PLACEMENT_3D('',#6691,#5556,#5557) ;
#4405 = AXIS2_PLACEMENT_3D('',#6697,#5561,#5562) ;
#4406 = AXIS2_PLACEMENT_3D('',#6703,#5566,#5567) ;
#4407 = AXIS2_PLACEMENT_3D('',#6709,#5571,#5572) ;
#4408 = AXIS2_PLACEMENT_3D('',#6713,#5575,#5576) ;
#4409 = AXIS2_PLACEMENT_3D('',#6717,#5579,#5580) ;
#4410 = AXIS2_PLACEMENT_3D('',#6719,#5582,#5583) ;
#4411 = AXIS2_PLACEMENT_3D('',#6721,#5584,#5585) ;
#4412 = AXIS2_PLACEMENT_3D('',#6722,#5586,#5587) ;
#4413 = AXIS2_PLACEMENT_3D('',#6724,#5588,#5589) ;
#4414 = AXIS2_PLACEMENT_3D('',#6726,#5590,#5591) ;
#4415 = AXIS2_PLACEMENT_3D('',#6727,#5592,#5593) ;
#4416 = AXIS2_PLACEMENT_3D('',#6729,#5594,#5595) ;
#4417 = AXIS2_PLACEMENT_3D('',#6730,#5596,#5597) ;
#4418 = AXIS2_PLACEMENT_3D('',#6732,#5598,#5599) ;
#4419 = AXIS2_PLACEMENT_3D('',#6733,#5600,#5601) ;
#4420 = AXIS2_PLACEMENT_3D('',#6734,#5602,#5603) ;
#4421 = AXIS2_PLACEMENT_3D('',#6736,#5605,#5606) ;
#4422 = AXIS2_PLACEMENT_3D('',#6738,#5607,#5608) ;
#4423 = AXIS2_PLACEMENT_3D('',#6739,#5609,#5610) ;
#4424 = AXIS2_PLACEMENT_3D('',#6740,#5611,#5612) ;
#4425 = AXIS2_PLACEMENT_3D('',#6743,#5614,#5615) ;
#4426 = AXIS2_PLACEMENT_3D('',#6744,#5616,#5617) ;
#4427 = AXIS2_PLACEMENT_3D('',#6746,#5619,#5620) ;
#4428 = AXIS2_PLACEMENT_3D('',#6747,#5621,#5622) ;
#4429 = AXIS2_PLACEMENT_3D('',#6748,#5623,#5624) ;
#4430 = AXIS2_PLACEMENT_3D('',#6749,#5625,#5626) ;
#4431 = AXIS2_PLACEMENT_3D('',#6750,#5627,#5628) ;
#4432 = AXIS2_PLACEMENT_3D('',#6751,#5629,#5630) ;
#4433 = AXIS2_PLACEMENT_3D('',#6752,#5631,#5632) ;
#4434 = AXIS2_PLACEMENT_3D('',#6753,#5633,#5634) ;
#4435 = AXIS2_PLACEMENT_3D('',#6754,#5635,#5636) ;
#4436 = AXIS2_PLACEMENT_3D('',#6755,#5637,#5638) ;
#4437 = DIRECTION('axis',(0.,0.,1.)) ;
#4438 = DIRECTION('refdir',(1.,0.,0.)) ;
#4439 = DIRECTION('axis',(0.,0.,1.)) ;
#4440 = DIRECTION('refdir',(1.,0.,0.)) ;
#4441 = DIRECTION('center_axis',(0.,0.,1.)) ;
#4442 = DIRECTION('ref_axis',(0.999199679743744,0.0399999999999898,0.)) ;
#4443 = DIRECTION('center_axis',(0.,0.,1.)) ;
#4444 = DIRECTION('ref_axis',(-1.,0.,0.)) ;
#4445 = DIRECTION('',(0.,0.,1.)) ;
#4446 = DIRECTION('center_axis',(0.,0.,1.)) ;
#4447 = DIRECTION('ref_axis',(-1.,0.,0.)) ;
#4448 = DIRECTION('',(0.,0.,1.)) ;
#4449 = DIRECTION('center_axis',(-5.3290705182E-15,2.6645352591E-15,-1.)) ;
#4450 = DIRECTION('ref_axis',(9.63812363252714E-14,1.,2.66453525909949E-15)) ;
#4451 = DIRECTION('center_axis',(3.49912784066E-16,5.43154451424E-16,1.)) ;
#4452 = DIRECTION('ref_axis',(-1.,1.113901422397E-48,3.49912784066E-16)) ;
#4453 = DIRECTION('center_axis',(-5.3290705182E-15,2.6645352591E-15,1.)) ;
#4454 = DIRECTION('ref_axis',(-9.67975699595058E-14,1.,-2.66453525910052E-15)) ;
#4455 = DIRECTION('center_axis',(-3.49912784066E-16,-5.43154451424E-16,1.)) ;
#4456 = DIRECTION('ref_axis',(-1.,1.113901422397E-48,-3.49912784066E-16)) ;
#4457 = DIRECTION('center_axis',(0.,1.,0.)) ;
#4458 = DIRECTION('ref_axis',(0.877582561890372,0.,-0.479425538604204)) ;
#4459 = DIRECTION('center_axis',(0.,1.,0.)) ;
#4460 = DIRECTION('ref_axis',(0.,0.,-1.)) ;
#4461 = DIRECTION('',(0.,1.,0.)) ;
#4462 = DIRECTION('center_axis',(0.,1.,0.)) ;
#4463 = DIRECTION('ref_axis',(0.,0.,-1.)) ;
#4464 = DIRECTION('center_axis',(-1.30266168223E-13,1.,1.71714494475E-13)) ;
#4465 = DIRECTION('ref_axis',(0.877582561890372,1.96643631636608E-13,-0.479425538604204)) ;
#4466 = DIRECTION('',(-0.62054458056418,0.707106781186018,0.339005049421354)) ;
#4467 = DIRECTION('center_axis',(4.23048538083E-14,1.,7.74385154649E-14)) ;
#4468 = DIRECTION('ref_axis',(4.65739899425144E-44,7.74385154649E-14,-1.)) ;
#4469 = DIRECTION('center_axis',(0.,1.,0.)) ;
#4470 = DIRECTION('ref_axis',(0.877582561890372,0.,-0.479425538604204)) ;
#4471 = DIRECTION('center_axis',(0.,1.,0.)) ;
#4472 = DIRECTION('ref_axis',(0.,0.,-1.)) ;
#4473 = DIRECTION('',(0.,1.,0.)) ;
#4474 = DIRECTION('center_axis',(0.,1.,0.)) ;
#4475 = DIRECTION('ref_axis',(0.,0.,-1.)) ;
#4476 = DIRECTION('center_axis',(-1.30266168223E-13,1.,1.74675089208E-13)) ;
#4477 = DIRECTION('ref_axis',(0.877582561890372,1.98063016361065E-13,-0.479425538604204)) ;
#4478 = DIRECTION('',(-0.62054458056418,0.707106781186017,0.339005049421356)) ;
#4479 = DIRECTION('center_axis',(4.35504810908E-14,1.,7.97186209114E-14)) ;
#4480 = DIRECTION('ref_axis',(2.58022100039044E-43,7.97186209114E-14,-1.)) ;
#4481 = DIRECTION('center_axis',(0.,1.,0.)) ;
#4482 = DIRECTION('ref_axis',(0.877582561890372,0.,-0.479425538604204)) ;
#4483 = DIRECTION('center_axis',(0.,1.,0.)) ;
#4484 = DIRECTION('ref_axis',(0.,0.,-1.)) ;
#4485 = DIRECTION('',(0.,1.,0.)) ;
#4486 = DIRECTION('center_axis',(0.,1.,0.)) ;
#4487 = DIRECTION('ref_axis',(0.,0.,-1.)) ;
#4488 = DIRECTION('center_axis',(-1.18423789293E-13,1.,1.7763568394E-13)) ;
#4489 = DIRECTION('ref_axis',(0.877582561890372,1.89089735844777E-13,-0.479425538604204)) ;
#4490 = DIRECTION('',(-0.620544580564171,0.707106781186024,0.339005049421358)) ;
#4491 = DIRECTION('center_axis',(4.75180655168E-14,1.,8.6981235488E-14)) ;
#4492 = DIRECTION('ref_axis',(-9.16589391413786E-44,8.6981235488E-14,-1.)) ;
#4493 = DIRECTION('center_axis',(0.,1.,0.)) ;
#4494 = DIRECTION('ref_axis',(0.877582561890372,0.,-0.479425538604204)) ;
#4495 = DIRECTION('center_axis',(0.,1.,0.)) ;
#4496 = DIRECTION('ref_axis',(0.,0.,-1.)) ;
#4497 = DIRECTION('',(0.,1.,0.)) ;
#4498 = DIRECTION('center_axis',(0.,1.,0.)) ;
#4499 = DIRECTION('ref_axis',(0.,0.,-1.)) ;
#4500 = DIRECTION('center_axis',(-1.18423789293E-13,1.,1.83556873405E-13)) ;
#4501 = DIRECTION('ref_axis',(0.877582561890372,1.91928505293212E-13,-0.479425538604204)) ;
#4502 = DIRECTION('',(-0.620544580564171,0.707106781186022,0.339005049421363)) ;
#4503 = DIRECTION('center_axis',(5.00093200818E-14,1.,9.15414463809E-14)) ;
#4504 = DIRECTION('ref_axis',(-7.43578035279155E-44,9.15414463809E-14,-1.)) ;
#4505 = DIRECTION('center_axis',(0.,0.,1.)) ;
#4506 = DIRECTION('ref_axis',(1.,0.,0.)) ;
#4507 = DIRECTION('',(1.,0.,0.)) ;
#4508 = DIRECTION('',(-1.,0.,0.)) ;
#4509 = DIRECTION('',(0.,1.,0.)) ;
#4510 = DIRECTION('center_axis',(-9.63097017110531E-7,6.43563312525601E-7,
-0.999999999999329)) ;
#4511 = DIRECTION('ref_axis',(-0.707106621415537,0.70710694095661,1.13608036309705E-6)) ;
#4512 = DIRECTION('',(0.707106781186548,0.707106781186548,0.)) ;
#4513 = DIRECTION('',(0.,1.,0.)) ;
#4514 = DIRECTION('',(0.707106781186548,-0.707106781186548,0.)) ;
#4515 = DIRECTION('',(1.,0.,0.)) ;
#4516 = DIRECTION('',(0.707106781186548,0.707106781186548,0.)) ;
#4517 = DIRECTION('center_axis',(2.25942303733386E-7,-1.13593817941397E-6,
-0.999999999999329)) ;
#4518 = DIRECTION('ref_axis',(-2.25947536598826E-7,-0.999999999999329,1.13593812836286E-6)) ;
#4519 = DIRECTION('',(1.,0.,0.)) ;
#4520 = DIRECTION('center_axis',(-6.43554037258066E-7,-9.63074619200789E-7,
-0.999999999999329)) ;
#4521 = DIRECTION('ref_axis',(-0.707106940950062,-0.707106621422085,1.13605796678281E-6)) ;
#4522 = DIRECTION('',(0.707106781186548,-0.707106781186548,0.)) ;
#4523 = DIRECTION('',(1.,0.,0.)) ;
#4524 = DIRECTION('',(-0.707106781186548,-0.707106781186548,0.)) ;
#4525 = DIRECTION('center_axis',(3.96642434162338E-7,-5.93533143460979E-7,
-0.999999999999745)) ;
#4526 = DIRECTION('ref_axis',(-3.24285719155748E-7,-0.999999999999771,5.93533014835517E-7)) ;
#4527 = DIRECTION('',(1.,0.,0.)) ;
#4528 = DIRECTION('center_axis',(-1.39239436415965E-7,-7.00115564002718E-7,
-0.999999999999745)) ;
#4529 = DIRECTION('ref_axis',(-0.707107010481907,-0.707106551890865,5.9351348401252E-7)) ;
#4530 = DIRECTION('',(-0.707106781186548,0.707106781186548,0.)) ;
#4531 = DIRECTION('',(1.,0.,0.)) ;
#4532 = DIRECTION('',(-0.707106781186548,-0.707106781186548,0.)) ;
#4533 = DIRECTION('',(0.,1.,0.)) ;
#4534 = DIRECTION('',(-0.707106781186548,0.707106781186548,0.)) ;
#4535 = DIRECTION('center_axis',(5.93533045622587E-7,3.96642398122336E-7,
-0.999999999999745)) ;
#4536 = DIRECTION('ref_axis',(0.999999999999771,-3.24285692193144E-7,5.93532916997148E-7)) ;
#4537 = DIRECTION('',(0.,1.,0.)) ;
#4538 = DIRECTION('center_axis',(-6.27646083255E-12,2.93098878501E-12,1.)) ;
#4539 = DIRECTION('ref_axis',(-0.987688340594861,-0.156434465041978,-5.74067952188287E-12)) ;
#4540 = DIRECTION('',(-0.707106781185048,1.4361112355401E-12,0.707106781188048)) ;
#4541 = DIRECTION('center_axis',(6.06458601694E-13,-3.82902891499E-12,-1.)) ;
#4542 = DIRECTION('ref_axis',(1.,1.11960132041635E-40,6.06458601694E-13)) ;
#4543 = DIRECTION('',(-0.50000000000309,0.49999999999609,0.707106781187127)) ;
#4544 = DIRECTION('center_axis',(0.49999999999984,-0.49999999999984,0.707106781186774)) ;
#4545 = DIRECTION('ref_axis',(0.707106781186547,0.707106781186548,3.33066907361881E-16)) ;
#4546 = DIRECTION('',(0.707106781186548,0.707106781186548,0.)) ;
#4547 = DIRECTION('',(-0.49999999999984,0.49999999999984,0.707106781186774)) ;
#4548 = DIRECTION('center_axis',(1.18423789293E-14,0.,-1.)) ;
#4549 = DIRECTION('ref_axis',(0.98768834059517,0.156434465040027,1.16965795933795E-14)) ;
#4550 = DIRECTION('center_axis',(2.89803640077E-16,-1.8297481715E-15,-1.)) ;
#4551 = DIRECTION('ref_axis',(1.,2.40832247656156E-47,2.89803640077E-16)) ;
#4552 = DIRECTION('',(0.707106781186548,0.,-0.707106781186548)) ;
#4553 = DIRECTION('center_axis',(0.707106781186548,0.,0.707106781186548)) ;
#4554 = DIRECTION('ref_axis',(0.,1.,0.)) ;
#4555 = DIRECTION('',(0.,1.,0.)) ;
#4556 = DIRECTION('',(-0.707106781186548,0.,0.707106781186548)) ;
#4557 = DIRECTION('center_axis',(-1.18423789293E-14,-1.18423789293E-14,-1.)) ;
#4558 = DIRECTION('ref_axis',(0.587785252292138,0.809016994375191,-1.65414614943321E-14)) ;
#4559 = DIRECTION('center_axis',(-2.11955181157E-15,1.53994453142E-15,-1.)) ;
#4560 = DIRECTION('ref_axis',(1.,-2.00835703363761E-46,-2.11955181157E-15)) ;
#4561 = DIRECTION('',(0.49999999999984,0.49999999999984,-0.707106781186774)) ;
#4562 = DIRECTION('center_axis',(-0.49999999999984,-0.49999999999984,-0.707106781186774)) ;
#4563 = DIRECTION('ref_axis',(0.707106781186547,-0.707106781186548,3.33066907361881E-16)) ;
#4564 = DIRECTION('',(0.707106781186548,-0.707106781186548,0.)) ;
#4565 = DIRECTION('',(-0.49999999999984,-0.49999999999984,0.707106781186774)) ;
#4566 = DIRECTION('center_axis',(0.,1.18423789293E-14,-1.)) ;
#4567 = DIRECTION('ref_axis',(-0.156434465040027,0.98768834059517,1.16965795933795E-14)) ;
#4568 = DIRECTION('center_axis',(1.8297481715E-15,2.89803640077E-16,-1.)) ;
#4569 = DIRECTION('ref_axis',(1.,-2.40832247656156E-47,1.8297481715E-15)) ;
#4570 = DIRECTION('',(0.,0.707106781186548,-0.707106781186548)) ;
#4571 = DIRECTION('center_axis',(0.,-0.707106781186548,-0.707106781186548)) ;
#4572 = DIRECTION('ref_axis',(1.,0.,0.)) ;
#4573 = DIRECTION('',(1.,0.,0.)) ;
#4574 = DIRECTION('',(0.,-0.707106781186548,0.707106781186548)) ;
#4575 = DIRECTION('center_axis',(1.18423789293E-14,-1.18423789293E-14,-1.)) ;
#4576 = DIRECTION('ref_axis',(-0.809016994375191,0.587785252292138,-1.65414614943321E-14)) ;
#4577 = DIRECTION('center_axis',(-1.53994453142E-15,-2.11955181157E-15,-1.)) ;
#4578 = DIRECTION('ref_axis',(1.,2.00835703363761E-46,-1.53994453142E-15)) ;
#4579 = DIRECTION('',(-0.49999999999984,0.49999999999984,-0.707106781186774)) ;
#4580 = DIRECTION('center_axis',(0.49999999999984,-0.49999999999984,-0.707106781186774)) ;
#4581 = DIRECTION('ref_axis',(0.707106781186547,0.707106781186548,-3.33066907361881E-16)) ;
#4582 = DIRECTION('',(0.707106781186548,0.707106781186548,0.)) ;
#4583 = DIRECTION('',(0.49999999999984,-0.49999999999984,0.707106781186774)) ;
#4584 = DIRECTION('center_axis',(2.37439697533E-12,-6.52515079006E-12,1.)) ;
#4585 = DIRECTION('ref_axis',(0.809016994376012,-0.587785252291009,-5.75631490780926E-12)) ;
#4586 = DIRECTION('center_axis',(2.28255961007E-12,3.14167377971E-12,-1.)) ;
#4587 = DIRECTION('ref_axis',(1.,-2.81265537546077E-40,2.28255961007E-12)) ;
#4588 = DIRECTION('',(4.97823982232033E-12,-0.707106781186048,0.707106781187048)) ;
#4589 = DIRECTION('center_axis',(0.,-0.707106781186548,-0.707106781186548)) ;
#4590 = DIRECTION('ref_axis',(1.,0.,0.)) ;
#4591 = DIRECTION('',(1.,0.,0.)) ;
#4592 = DIRECTION('',(0.,-0.707106781186548,0.707106781186548)) ;
#4593 = DIRECTION('center_axis',(-2.93394937974E-12,-6.28830321148E-12,1.)) ;
#4594 = DIRECTION('ref_axis',(0.156434465041978,-0.987688340594861,-5.75191296242415E-12)) ;
#4595 = DIRECTION('center_axis',(3.83374680699E-12,6.07205842377E-13,-1.)) ;
#4596 = DIRECTION('ref_axis',(1.,-1.49541384440967E-40,3.83374680699E-12)) ;
#4597 = DIRECTION('',(-0.49999999999609,-0.50000000000309,0.707106781187127)) ;
#4598 = DIRECTION('center_axis',(-0.49999999999984,-0.49999999999984,-0.707106781186774)) ;
#4599 = DIRECTION('ref_axis',(0.707106781186547,-0.707106781186548,3.33066907361881E-16)) ;
#4600 = DIRECTION('',(0.707106781186548,-0.707106781186548,0.)) ;
#4601 = DIRECTION('',(-0.49999999999984,-0.49999999999984,0.707106781186774)) ;
#4602 = DIRECTION('center_axis',(2.96059473233E-15,1.18423789293E-14,-1.)) ;
#4603 = DIRECTION('ref_axis',(-0.156434465040027,0.98768834059517,1.12334405402272E-14)) ;
#4604 = DIRECTION('center_axis',(4.71789199381E-15,7.47240682951E-16,-1.)) ;
#4605 = DIRECTION('ref_axis',(1.,-2.48107229741873E-46,4.71789199381E-15)) ;
#4606 = DIRECTION('',(-2.09345661157866E-15,0.707106781186548,-0.707106781186548)) ;
#4607 = DIRECTION('center_axis',(0.,-0.707106781186548,-0.707106781186548)) ;
#4608 = DIRECTION('ref_axis',(1.,0.,0.)) ;
#4609 = DIRECTION('',(1.,0.,0.)) ;
#4610 = DIRECTION('',(0.,-0.707106781186548,0.707106781186548)) ;
#4611 = DIRECTION('center_axis',(-5.92118946467E-15,2.36847578587E-14,-1.)) ;
#4612 = DIRECTION('ref_axis',(-0.809016994375191,0.587785252292138,1.87118942772875E-14)) ;
#4613 = DIRECTION('center_axis',(9.21705100259E-15,1.268618236E-14,-1.)) ;
#4614 = DIRECTION('ref_axis',(1.,-1.19244796912461E-45,9.21705100259E-15)) ;
#4615 = DIRECTION('',(-0.49999999999984,0.49999999999984,-0.707106781186774)) ;
#4616 = DIRECTION('center_axis',(-0.49999999999984,0.49999999999984,0.707106781186774)) ;
#4617 = DIRECTION('ref_axis',(-0.707106781186547,-0.707106781186548,3.33066907361881E-16)) ;
#4618 = DIRECTION('',(-0.707106781186548,-0.707106781186548,0.)) ;
#4619 = DIRECTION('',(0.49999999999984,-0.49999999999984,0.707106781186774)) ;
#4620 = DIRECTION('center_axis',(-1.48029736617E-14,3.5527136788E-14,1.)) ;
#4621 = DIRECTION('ref_axis',(0.707106781186548,-0.707106781186548,3.55887623968508E-14)) ;
#4622 = DIRECTION('center_axis',(-1.03620815632E-14,-1.03620815632E-14,-1.)) ;
#4623 = DIRECTION('ref_axis',(1.,7.78499045260793E-45,-1.03620815632E-14)) ;
#4624 = DIRECTION('',(-3.34953057852786E-14,-0.707106781186548,0.707106781186548)) ;
#4625 = DIRECTION('center_axis',(0.,-0.707106781186548,-0.707106781186548)) ;
#4626 = DIRECTION('ref_axis',(1.,0.,0.)) ;
#4627 = DIRECTION('',(1.,0.,0.)) ;
#4628 = DIRECTION('',(0.,-0.707106781186548,0.707106781186548)) ;
#4629 = DIRECTION('center_axis',(5.92118946467E-15,1.18423789293E-14,1.)) ;
#4630 = DIRECTION('ref_axis',(0.156434465040027,-0.98768834059517,1.07703014870732E-14)) ;
#4631 = DIRECTION('center_axis',(-7.60603581612E-15,-1.20467772583E-15,-1.)) ;
#4632 = DIRECTION('ref_axis',(1.,5.2570604439658E-46,-7.60603581612E-15)) ;
#4633 = DIRECTION('',(-0.49999999999984,-0.49999999999984,0.707106781186774)) ;
#4634 = DIRECTION('center_axis',(0.49999999999984,0.49999999999984,0.707106781186774)) ;
#4635 = DIRECTION('ref_axis',(-0.707106781186547,0.707106781186548,-3.33066907361881E-16)) ;
#4636 = DIRECTION('',(-0.707106781186548,0.707106781186548,0.)) ;
#4637 = DIRECTION('',(-0.49999999999984,-0.49999999999984,0.707106781186774)) ;
#4638 = DIRECTION('center_axis',(1.18423789293E-14,4.73695157173E-14,-1.)) ;
#4639 = DIRECTION('ref_axis',(-0.156434465040027,0.98768834059517,4.49337621610105E-14)) ;
#4640 = DIRECTION('center_axis',(1.88715679752E-14,2.98896273181E-15,-1.)) ;
#4641 = DIRECTION('ref_axis',(1.,-3.73441846949733E-45,1.88715679752E-14)) ;
#4642 = DIRECTION('',(-8.37382644630462E-15,0.707106781186548,-0.707106781186548)) ;
#4643 = DIRECTION('center_axis',(0.,-0.707106781186548,-0.707106781186548)) ;
#4644 = DIRECTION('ref_axis',(1.,0.,0.)) ;
#4645 = DIRECTION('',(1.,0.,0.)) ;
#4646 = DIRECTION('',(0.,-0.707106781186548,0.707106781186548)) ;
#4647 = DIRECTION('center_axis',(-1.18423789293E-14,3.5527136788E-14,-1.)) ;
#4648 = DIRECTION('ref_axis',(-0.809016994375191,0.587785252292138,3.04630128677863E-14)) ;
#4649 = DIRECTION('center_axis',(1.28027161806E-14,1.76214270839E-14,-1.)) ;
#4650 = DIRECTION('ref_axis',(1.,-3.57263571433164E-45,1.28027161806E-14)) ;
#4651 = DIRECTION('',(-0.49999999999984,0.49999999999984,-0.707106781186774)) ;
#4652 = DIRECTION('center_axis',(-0.49999999999984,0.49999999999984,0.707106781186774)) ;
#4653 = DIRECTION('ref_axis',(-0.707106781186547,-0.707106781186548,3.33066907361881E-16)) ;
#4654 = DIRECTION('',(-0.707106781186548,-0.707106781186548,0.)) ;
#4655 = DIRECTION('',(0.49999999999984,-0.49999999999984,0.707106781186774)) ;
#4656 = DIRECTION('center_axis',(-4.73695157173E-14,1.18423789293E-14,-1.)) ;
#4657 = DIRECTION('ref_axis',(-0.98768834059517,-0.156434465040027,4.49337621610105E-14)) ;
#4658 = DIRECTION('center_axis',(-2.98896273181E-15,1.88715679752E-14,-1.)) ;
#4659 = DIRECTION('ref_axis',(1.,3.73441846949733E-45,-2.98896273181E-15)) ;
#4660 = DIRECTION('',(-0.707106781186548,-8.37382644630462E-15,-0.707106781186548)) ;
#4661 = DIRECTION('center_axis',(0.707106781186548,0.,-0.707106781186548)) ;
#4662 = DIRECTION('ref_axis',(0.,1.,0.)) ;
#4663 = DIRECTION('',(0.,1.,0.)) ;
#4664 = DIRECTION('',(0.707106781186548,0.,0.707106781186548)) ;
#4665 = DIRECTION('center_axis',(-1.18423789293E-14,0.,-1.)) ;
#4666 = DIRECTION('ref_axis',(-0.587785252292138,-0.809016994375191,6.9607756866977E-15)) ;
#4667 = DIRECTION('center_axis',(-7.75093763616E-15,5.63138582459E-15,-1.)) ;
#4668 = DIRECTION('ref_axis',(1.,1.34620891396805E-45,-7.75093763616E-15)) ;
#4669 = DIRECTION('',(-0.49999999999984,-0.49999999999984,-0.707106781186774)) ;
#4670 = DIRECTION('center_axis',(0.49999999999984,0.49999999999984,-0.707106781186774)) ;
#4671 = DIRECTION('ref_axis',(-0.707106781186547,0.707106781186548,3.33066907361881E-16)) ;
#4672 = DIRECTION('',(-0.707106781186548,0.707106781186548,0.)) ;
#4673 = DIRECTION('',(0.49999999999984,0.49999999999984,0.707106781186774)) ;
#4674 = DIRECTION('center_axis',(-2.36847578587E-14,-1.18423789293E-14,1.)) ;
#4675 = DIRECTION('ref_axis',(0.707106781186548,0.707106781186548,2.51214793389369E-14)) ;
#4676 = DIRECTION('center_axis',(5.92118946467E-15,-5.92118946467E-15,-1.)) ;
#4677 = DIRECTION('ref_axis',(1.,6.22799323720626E-46,5.92118946467E-15)) ;
#4678 = DIRECTION('',(0.707106781186548,-3.97756756199745E-14,0.707106781186548)) ;
#4679 = DIRECTION('center_axis',(0.707106781186548,0.,-0.707106781186548)) ;
#4680 = DIRECTION('ref_axis',(0.,1.,0.)) ;
#4681 = DIRECTION('',(0.707106781186548,0.,0.707106781186548)) ;
#4682 = DIRECTION('',(0.,1.,0.)) ;
#4683 = DIRECTION('center_axis',(0.707106781186548,0.,0.707106781186548)) ;
#4684 = DIRECTION('ref_axis',(0.,1.,0.)) ;
#4685 = DIRECTION('',(0.,1.,0.)) ;
#4686 = DIRECTION('',(-0.707106781186548,0.,0.707106781186548)) ;
#4687 = DIRECTION('center_axis',(0.,0.,1.)) ;
#4688 = DIRECTION('ref_axis',(1.,0.,0.)) ;
#4689 = DIRECTION('',(0.,1.,0.)) ;
#4690 = DIRECTION('center_axis',(-5.9353304562263E-7,-3.96642398122351E-7,
-0.999999999999745)) ;
#4691 = DIRECTION('ref_axis',(0.999999999999771,-3.24285666816574E-7,-5.93532916997201E-7)) ;
#4692 = DIRECTION('',(-0.707106781186548,0.707106781186548,0.)) ;
#4693 = DIRECTION('',(0.,1.,0.)) ;
#4694 = DIRECTION('',(-0.707106781186548,-0.707106781186548,0.)) ;
#4695 = DIRECTION('',(1.,0.,0.)) ;
#4696 = DIRECTION('',(-0.707106781186548,0.707106781186548,0.)) ;
#4697 = DIRECTION('center_axis',(1.39239491916582E-7,7.00115676332798E-7,
-0.999999999999745)) ;
#4698 = DIRECTION('ref_axis',(-0.707107010481932,-0.707106551890839,-5.93513602686716E-7)) ;
#4699 = DIRECTION('',(1.,0.,0.)) ;
#4700 = DIRECTION('center_axis',(-3.96642440063609E-7,5.93533152292858E-7,
-0.999999999999745)) ;
#4701 = DIRECTION('ref_axis',(-3.24285714397637E-7,-0.999999999999771,-5.93533023667397E-7)) ;
#4702 = DIRECTION('',(-0.707106781186548,-0.707106781186548,0.)) ;
#4703 = DIRECTION('',(1.,0.,0.)) ;
#4704 = DIRECTION('',(0.707106781186548,-0.707106781186548,0.)) ;
#4705 = DIRECTION('center_axis',(6.4354811537276E-7,9.63053640304665E-7,-0.999999999999329)) ;
#4706 = DIRECTION('ref_axis',(-0.707106940957591,-0.707106621414556,-1.13603894505784E-6)) ;
#4707 = DIRECTION('',(1.,0.,0.)) ;
#4708 = DIRECTION('center_axis',(-2.25931656503166E-7,1.13591913526646E-6,
-0.999999999999329)) ;
#4709 = DIRECTION('ref_axis',(-2.25958188412347E-7,-0.999999999999329,-1.13591908421535E-6)) ;
#4710 = DIRECTION('',(0.707106781186548,0.707106781186548,0.)) ;
#4711 = DIRECTION('',(1.,0.,0.)) ;
#4712 = DIRECTION('',(0.707106781186548,-0.707106781186548,0.)) ;
#4713 = DIRECTION('',(0.,1.,0.)) ;
#4714 = DIRECTION('',(0.707106781186548,0.707106781186548,0.)) ;
#4715 = DIRECTION('center_axis',(9.63097017110531E-7,-6.43563312525601E-7,
-0.999999999999329)) ;
#4716 = DIRECTION('ref_axis',(-0.707106621415537,0.70710694095661,-1.13608036309705E-6)) ;
#4717 = DIRECTION('',(0.,1.,0.)) ;
#4718 = DIRECTION('',(-1.,0.,0.)) ;
#4719 = DIRECTION('',(1.,0.,0.)) ;
#4720 = DIRECTION('center_axis',(0.,0.,1.)) ;
#4721 = DIRECTION('ref_axis',(0.,-1.,0.)) ;
#4722 = DIRECTION('center_axis',(0.,0.,1.)) ;
#4723 = DIRECTION('ref_axis',(-1.,0.,0.)) ;
#4724 = DIRECTION('',(0.,0.,1.)) ;
#4725 = DIRECTION('',(0.,0.,1.)) ;
#4726 = DIRECTION('center_axis',(0.,0.,1.)) ;
#4727 = DIRECTION('ref_axis',(-0.707106781186548,-0.707106781186548,0.)) ;
#4728 = DIRECTION('center_axis',(0.,0.,1.)) ;
#4729 = DIRECTION('ref_axis',(-1.,0.,0.)) ;
#4730 = DIRECTION('',(0.,0.,1.)) ;
#4731 = DIRECTION('',(0.,0.,1.)) ;
#4732 = DIRECTION('center_axis',(0.,0.,1.)) ;
#4733 = DIRECTION('ref_axis',(0.,-1.,0.)) ;
#4734 = DIRECTION('center_axis',(0.,0.,1.)) ;
#4735 = DIRECTION('ref_axis',(-1.,0.,0.)) ;
#4736 = DIRECTION('',(0.,0.,1.)) ;
#4737 = DIRECTION('',(0.,0.,1.)) ;
#4738 = DIRECTION('center_axis',(0.,0.,1.)) ;
#4739 = DIRECTION('ref_axis',(-0.707106781186548,-0.707106781186548,0.)) ;
#4740 = DIRECTION('center_axis',(0.,0.,1.)) ;
#4741 = DIRECTION('ref_axis',(-1.,0.,0.)) ;
#4742 = DIRECTION('',(0.,0.,1.)) ;
#4743 = DIRECTION('',(0.,0.,1.)) ;
#4744 = DIRECTION('center_axis',(0.,0.,1.)) ;
#4745 = DIRECTION('ref_axis',(1.,0.,0.)) ;
#4746 = DIRECTION('center_axis',(0.,0.,1.)) ;
#4747 = DIRECTION('ref_axis',(-1.,0.,0.)) ;
#4748 = DIRECTION('',(0.,0.,1.)) ;
#4749 = DIRECTION('',(0.,0.,1.)) ;
#4750 = DIRECTION('center_axis',(0.,0.,1.)) ;
#4751 = DIRECTION('ref_axis',(-0.707106781186548,0.707106781186548,0.)) ;
#4752 = DIRECTION('center_axis',(0.,0.,1.)) ;
#4753 = DIRECTION('ref_axis',(-1.,0.,0.)) ;
#4754 = DIRECTION('',(0.,0.,1.)) ;
#4755 = DIRECTION('',(0.,0.,1.)) ;
#4756 = DIRECTION('center_axis',(-1.,0.,0.)) ;
#4757 = DIRECTION('ref_axis',(0.,-1.,0.)) ;
#4758 = DIRECTION('',(0.,1.,0.)) ;
#4759 = DIRECTION('',(0.,0.,1.)) ;
#4760 = DIRECTION('center_axis',(0.,1.,0.)) ;
#4761 = DIRECTION('ref_axis',(-1.,0.,0.)) ;
#4762 = DIRECTION('',(1.,0.,0.)) ;
#4763 = DIRECTION('center_axis',(0.,1.,0.)) ;
#4764 = DIRECTION('ref_axis',(-1.,0.,0.)) ;
#4765 = DIRECTION('',(1.,0.,0.)) ;
#4766 = DIRECTION('center_axis',(-1.,0.,0.)) ;
#4767 = DIRECTION('ref_axis',(0.,-1.,0.)) ;
#4768 = DIRECTION('',(0.,0.,1.)) ;
#4769 = DIRECTION('',(0.,1.,0.)) ;
#4770 = DIRECTION('center_axis',(0.,-1.,0.)) ;
#4771 = DIRECTION('ref_axis',(1.,0.,0.)) ;
#4772 = DIRECTION('',(-0.707106781186548,0.,-0.707106781186548)) ;
#4773 = DIRECTION('center_axis',(0.,-1.,0.)) ;
#4774 = DIRECTION('ref_axis',(1.,0.,0.)) ;
#4775 = DIRECTION('',(0.707106781186548,0.,-0.707106781186548)) ;
#4776 = DIRECTION('center_axis',(0.,0.,1.)) ;
#4777 = DIRECTION('ref_axis',(1.,-2.22044604925E-16,0.)) ;
#4778 = DIRECTION('',(0.,0.,1.)) ;
#4779 = DIRECTION('',(0.,0.,1.)) ;
#4780 = DIRECTION('center_axis',(0.,0.,1.)) ;
#4781 = DIRECTION('ref_axis',(-1.,0.,0.)) ;
#4782 = DIRECTION('center_axis',(0.707106781186548,0.707106781186548,0.)) ;
#4783 = DIRECTION('ref_axis',(-0.707106781186548,0.707106781186548,0.)) ;
#4784 = DIRECTION('',(0.,0.,1.)) ;
#4785 = DIRECTION('',(0.707106781186548,-0.707106781186548,0.)) ;
#4786 = DIRECTION('center_axis',(0.,0.,1.)) ;
#4787 = DIRECTION('ref_axis',(0.707106781186547,0.707106781186547,0.)) ;
#4788 = DIRECTION('',(0.,0.,1.)) ;
#4789 = DIRECTION('center_axis',(0.,0.,1.)) ;
#4790 = DIRECTION('ref_axis',(-1.,0.,0.)) ;
#4791 = DIRECTION('center_axis',(-0.707106781186548,0.707106781186548,0.)) ;
#4792 = DIRECTION('ref_axis',(-0.707106781186548,-0.707106781186548,0.)) ;
#4793 = DIRECTION('',(0.,0.,1.)) ;
#4794 = DIRECTION('',(0.707106781186548,0.707106781186548,0.)) ;
#4795 = DIRECTION('center_axis',(0.,1.,0.)) ;
#4796 = DIRECTION('ref_axis',(-1.,0.,0.)) ;
#4797 = DIRECTION('',(0.,0.,1.)) ;
#4798 = DIRECTION('',(1.,0.,0.)) ;
#4799 = DIRECTION('center_axis',(0.,0.,1.)) ;
#4800 = DIRECTION('ref_axis',(2.22044604925E-16,1.,0.)) ;
#4801 = DIRECTION('center_axis',(0.,0.,1.)) ;
#4802 = DIRECTION('ref_axis',(-1.,0.,0.)) ;
#4803 = DIRECTION('center_axis',(0.707106781186548,0.707106781186548,0.)) ;
#4804 = DIRECTION('ref_axis',(-0.707106781186548,0.707106781186548,0.)) ;
#4805 = DIRECTION('',(0.,0.,1.)) ;
#4806 = DIRECTION('',(0.707106781186548,-0.707106781186548,0.)) ;
#4807 = DIRECTION('center_axis',(0.,0.,1.)) ;
#4808 = DIRECTION('ref_axis',(0.707106781186547,0.707106781186547,0.)) ;
#4809 = DIRECTION('',(0.,0.,1.)) ;
#4810 = DIRECTION('center_axis',(0.,0.,1.)) ;
#4811 = DIRECTION('ref_axis',(-1.,0.,0.)) ;
#4812 = DIRECTION('center_axis',(0.707106781186548,-0.707106781186548,0.)) ;
#4813 = DIRECTION('ref_axis',(0.707106781186548,0.707106781186548,0.)) ;
#4814 = DIRECTION('',(-0.707106781186548,-0.707106781186548,0.)) ;
#4815 = DIRECTION('',(0.,0.,1.)) ;
#4816 = DIRECTION('center_axis',(0.,1.,0.)) ;
#4817 = DIRECTION('ref_axis',(-1.,0.,0.)) ;
#4818 = DIRECTION('',(0.,0.,1.)) ;
#4819 = DIRECTION('',(1.,0.,0.)) ;
#4820 = DIRECTION('center_axis',(0.,0.,1.)) ;
#4821 = DIRECTION('ref_axis',(-2.22044604925E-16,1.,0.)) ;
#4822 = DIRECTION('center_axis',(0.,0.,1.)) ;
#4823 = DIRECTION('ref_axis',(-1.,0.,0.)) ;
#4824 = DIRECTION('center_axis',(-0.707106781186548,-0.707106781186548,0.)) ;
#4825 = DIRECTION('ref_axis',(0.707106781186548,-0.707106781186548,0.)) ;
#4826 = DIRECTION('',(-0.707106781186548,0.707106781186548,0.)) ;
#4827 = DIRECTION('',(0.,0.,1.)) ;
#4828 = DIRECTION('center_axis',(0.,0.,1.)) ;
#4829 = DIRECTION('ref_axis',(0.707106781186547,0.707106781186547,0.)) ;
#4830 = DIRECTION('',(0.,0.,1.)) ;
#4831 = DIRECTION('center_axis',(0.,0.,1.)) ;
#4832 = DIRECTION('ref_axis',(-1.,0.,0.)) ;
#4833 = DIRECTION('center_axis',(0.,1.,0.)) ;
#4834 = DIRECTION('ref_axis',(-1.,0.,0.)) ;
#4835 = DIRECTION('',(0.,0.,1.)) ;
#4836 = DIRECTION('',(1.,0.,0.)) ;
#4837 = DIRECTION('center_axis',(0.,0.,1.)) ;
#4838 = DIRECTION('ref_axis',(-1.14352971536E-14,1.,0.)) ;
#4839 = DIRECTION('',(0.,0.,1.)) ;
#4840 = DIRECTION('center_axis',(0.,0.,1.)) ;
#4841 = DIRECTION('ref_axis',(-1.,0.,0.)) ;
#4842 = DIRECTION('center_axis',(0.707106781186548,-0.707106781186548,0.)) ;
#4843 = DIRECTION('ref_axis',(0.707106781186548,0.707106781186548,0.)) ;
#4844 = DIRECTION('',(-0.707106781186548,-0.707106781186548,0.)) ;
#4845 = DIRECTION('',(0.,0.,1.)) ;
#4846 = DIRECTION('center_axis',(0.,0.,1.)) ;
#4847 = DIRECTION('ref_axis',(-0.707106781186547,0.707106781186547,0.)) ;
#4848 = DIRECTION('',(0.,0.,1.)) ;
#4849 = DIRECTION('center_axis',(0.,0.,1.)) ;
#4850 = DIRECTION('ref_axis',(-1.,0.,0.)) ;
#4851 = DIRECTION('center_axis',(-0.707106781186548,0.707106781186548,0.)) ;
#4852 = DIRECTION('ref_axis',(-0.707106781186548,-0.707106781186548,0.)) ;
#4853 = DIRECTION('',(0.707106781186548,0.707106781186548,0.)) ;
#4854 = DIRECTION('',(0.,0.,1.)) ;
#4855 = DIRECTION('center_axis',(-1.,0.,0.)) ;
#4856 = DIRECTION('ref_axis',(0.,-1.,0.)) ;
#4857 = DIRECTION('',(0.,1.,0.)) ;
#4858 = DIRECTION('',(0.,0.,1.)) ;
#4859 = DIRECTION('center_axis',(0.,0.,1.)) ;
#4860 = DIRECTION('ref_axis',(0.707106781186547,-0.707106781186547,0.)) ;
#4861 = DIRECTION('center_axis',(0.,0.,1.)) ;
#4862 = DIRECTION('ref_axis',(-1.,0.,0.)) ;
#4863 = DIRECTION('center_axis',(-0.707106781186548,-0.707106781186548,0.)) ;
#4864 = DIRECTION('ref_axis',(0.707106781186548,-0.707106781186548,0.)) ;
#4865 = DIRECTION('',(0.,0.,1.)) ;
#4866 = DIRECTION('',(-0.707106781186548,0.707106781186548,0.)) ;
#4867 = DIRECTION('center_axis',(-1.,0.,0.)) ;
#4868 = DIRECTION('ref_axis',(0.,-1.,0.)) ;
#4869 = DIRECTION('',(0.,0.,1.)) ;
#4870 = DIRECTION('',(0.,1.,0.)) ;
#4871 = DIRECTION('center_axis',(0.,0.,1.)) ;
#4872 = DIRECTION('ref_axis',(-1.,2.22044604925E-16,0.)) ;
#4873 = DIRECTION('center_axis',(0.,0.,1.)) ;
#4874 = DIRECTION('ref_axis',(-1.,0.,0.)) ;
#4875 = DIRECTION('center_axis',(-6.27646083255E-12,2.93098878501E-12,-1.)) ;
#4876 = DIRECTION('ref_axis',(-0.987688340594861,-0.156434465041978,5.74067952188287E-12)) ;
#4877 = DIRECTION('',(-0.707106781185044,-1.06686070120007E-7,-0.707106781188043)) ;
#4878 = DIRECTION('',(-0.50000000000284,0.49999999999684,-0.707106781186774)) ;
#4879 = DIRECTION('center_axis',(-0.49999999999984,0.49999999999984,0.707106781186774)) ;
#4880 = DIRECTION('ref_axis',(0.707106781186547,0.707106781186548,-3.33066907361881E-16)) ;
#4881 = DIRECTION('',(-0.49999999999984,0.49999999999984,-0.707106781186774)) ;
#4882 = DIRECTION('center_axis',(1.18423789293E-14,0.,1.)) ;
#4883 = DIRECTION('ref_axis',(0.98768834059517,0.156434465040027,-1.16965795933795E-14)) ;
#4884 = DIRECTION('',(0.707106781186548,0.,0.707106781186548)) ;
#4885 = DIRECTION('center_axis',(-0.707106781186548,0.,0.707106781186548)) ;
#4886 = DIRECTION('ref_axis',(0.,1.,0.)) ;
#4887 = DIRECTION('',(-0.707106781186548,0.,-0.707106781186548)) ;
#4888 = DIRECTION('center_axis',(-1.18423789293E-14,-1.18423789293E-14,1.)) ;
#4889 = DIRECTION('ref_axis',(0.587785252292138,0.809016994375191,1.65414614943321E-14)) ;
#4890 = DIRECTION('',(0.49999999999984,0.49999999999984,0.707106781186774)) ;
#4891 = DIRECTION('center_axis',(0.49999999999984,0.49999999999984,-0.707106781186774)) ;
#4892 = DIRECTION('ref_axis',(0.707106781186547,-0.707106781186548,-3.33066907361881E-16)) ;
#4893 = DIRECTION('',(-0.49999999999984,-0.49999999999984,-0.707106781186774)) ;
#4894 = DIRECTION('center_axis',(0.,1.18423789293E-14,1.)) ;
#4895 = DIRECTION('ref_axis',(-0.156434465040027,0.98768834059517,-1.16965795933795E-14)) ;
#4896 = DIRECTION('',(0.,0.707106781186548,0.707106781186548)) ;
#4897 = DIRECTION('center_axis',(0.,0.707106781186548,-0.707106781186548)) ;
#4898 = DIRECTION('ref_axis',(1.,0.,0.)) ;
#4899 = DIRECTION('',(0.,-0.707106781186548,-0.707106781186548)) ;
#4900 = DIRECTION('center_axis',(1.18423789293E-14,-1.18423789293E-14,1.)) ;
#4901 = DIRECTION('ref_axis',(-0.809016994375191,0.587785252292138,1.65414614943321E-14)) ;
#4902 = DIRECTION('',(-0.49999999999984,0.49999999999984,0.707106781186774)) ;
#4903 = DIRECTION('center_axis',(-0.49999999999984,0.49999999999984,-0.707106781186774)) ;
#4904 = DIRECTION('ref_axis',(0.707106781186547,0.707106781186548,3.33066907361881E-16)) ;
#4905 = DIRECTION('',(0.49999999999984,-0.49999999999984,-0.707106781186774)) ;
#4906 = DIRECTION('center_axis',(1.30266168223E-11,-2.55795384874E-11,-1.)) ;
#4907 = DIRECTION('ref_axis',(0.809016994378129,-0.587785252288094,2.55740298717221E-11)) ;
#4908 = DIRECTION('',(1.98962116363013E-11,-0.707106781181048,-0.707106781192048)) ;
#4909 = DIRECTION('center_axis',(0.,0.707106781186548,-0.707106781186548)) ;
#4910 = DIRECTION('ref_axis',(1.,0.,0.)) ;
#4911 = DIRECTION('',(0.,-0.707106781186548,-0.707106781186548)) ;
#4912 = DIRECTION('center_axis',(-8.86698122334E-12,-2.72966834321E-11,-1.)) ;
#4913 = DIRECTION('ref_axis',(0.156434465046035,-0.987688340594219,2.55735144985301E-11)) ;
#4914 = DIRECTION('',(-0.499999999982072,-0.500000000010072,-0.707106781192102)) ;
#4915 = DIRECTION('center_axis',(0.49999999999984,0.49999999999984,-0.707106781186774)) ;
#4916 = DIRECTION('ref_axis',(0.707106781186547,-0.707106781186548,-3.33066907361881E-16)) ;
#4917 = DIRECTION('',(-0.49999999999984,-0.49999999999984,-0.707106781186774)) ;
#4918 = DIRECTION('center_axis',(2.96059473233E-15,1.18423789293E-14,1.)) ;
#4919 = DIRECTION('ref_axis',(-0.156434465040027,0.98768834059517,-1.12334405402272E-14)) ;
#4920 = DIRECTION('',(-2.09345661157866E-15,0.707106781186548,0.707106781186548)) ;
#4921 = DIRECTION('center_axis',(0.,0.707106781186548,-0.707106781186548)) ;
#4922 = DIRECTION('ref_axis',(1.,0.,0.)) ;
#4923 = DIRECTION('',(0.,-0.707106781186548,-0.707106781186548)) ;
#4924 = DIRECTION('center_axis',(-5.92118946467E-15,2.36847578587E-14,1.)) ;
#4925 = DIRECTION('ref_axis',(-0.809016994375191,0.587785252292138,-1.87118942772875E-14)) ;
#4926 = DIRECTION('',(-0.49999999999984,0.49999999999984,0.707106781186774)) ;
#4927 = DIRECTION('center_axis',(0.49999999999984,-0.49999999999984,0.707106781186774)) ;
#4928 = DIRECTION('ref_axis',(-0.707106781186547,-0.707106781186548,-3.33066907361881E-16)) ;
#4929 = DIRECTION('',(0.49999999999984,-0.49999999999984,-0.707106781186774)) ;
#4930 = DIRECTION('center_axis',(-1.18423789293E-14,2.36847578587E-14,-1.)) ;
#4931 = DIRECTION('ref_axis',(0.809016994375191,-0.587785252292138,-2.35022371810886E-14)) ;
#4932 = DIRECTION('',(5.11457513742672E-8,-0.707106781186547,-0.707106781186547)) ;
#4933 = DIRECTION('center_axis',(0.,0.707106781186548,-0.707106781186548)) ;
#4934 = DIRECTION('ref_axis',(1.,0.,0.)) ;
#4935 = DIRECTION('',(0.,-0.707106781186548,-0.707106781186548)) ;
#4936 = DIRECTION('center_axis',(1.7763568394E-14,2.36847578587E-14,-1.)) ;
#4937 = DIRECTION('ref_axis',(0.156434465040027,-0.98768834059517,-2.06143248679405E-14)) ;
#4938 = DIRECTION('',(-0.499999963833839,-0.500000036165839,-0.707106781186773)) ;
#4939 = DIRECTION('center_axis',(-0.49999999999984,-0.49999999999984,0.707106781186774)) ;
#4940 = DIRECTION('ref_axis',(-0.707106781186547,0.707106781186548,3.33066907361881E-16)) ;
#4941 = DIRECTION('',(-0.49999999999984,-0.49999999999984,-0.707106781186774)) ;
#4942 = DIRECTION('center_axis',(-1.18423789293E-14,-1.18423789293E-14,1.)) ;
#4943 = DIRECTION('ref_axis',(-0.156434465040027,0.98768834059517,9.84402338077319E-15)) ;
#4944 = DIRECTION('',(-4.18691322315732E-15,0.707106781186548,0.707106781186548)) ;
#4945 = DIRECTION('center_axis',(0.,0.707106781186548,-0.707106781186548)) ;
#4946 = DIRECTION('ref_axis',(1.,0.,0.)) ;
#4947 = DIRECTION('',(0.,-0.707106781186548,-0.707106781186548)) ;
#4948 = DIRECTION('center_axis',(-1.18423789293E-14,3.5527136788E-14,1.)) ;
#4949 = DIRECTION('ref_axis',(-0.809016994375191,0.587785252292138,-3.04630128677863E-14)) ;
#4950 = DIRECTION('',(-0.49999999999984,0.49999999999984,0.707106781186774)) ;
#4951 = DIRECTION('center_axis',(0.49999999999984,-0.49999999999984,0.707106781186774)) ;
#4952 = DIRECTION('ref_axis',(-0.707106781186547,-0.707106781186548,-3.33066907361881E-16)) ;
#4953 = DIRECTION('',(0.49999999999984,-0.49999999999984,-0.707106781186774)) ;
#4954 = DIRECTION('center_axis',(1.18423789293E-14,-5.92118946467E-15,1.)) ;
#4955 = DIRECTION('ref_axis',(-0.98768834059517,-0.156434465040027,1.07703014870732E-14)) ;
#4956 = DIRECTION('',(-0.707106781186548,-4.18691322315732E-15,0.707106781186548)) ;
#4957 = DIRECTION('center_axis',(-0.707106781186548,0.,-0.707106781186548)) ;
#4958 = DIRECTION('ref_axis',(0.,1.,0.)) ;
#4959 = DIRECTION('',(0.707106781186548,0.,-0.707106781186548)) ;
#4960 = DIRECTION('center_axis',(-1.18423789293E-14,0.,1.)) ;
#4961 = DIRECTION('ref_axis',(-0.587785252292138,-0.809016994375191,-6.9607756866977E-15)) ;
#4962 = DIRECTION('',(-0.49999999999984,-0.49999999999984,0.707106781186774)) ;
#4963 = DIRECTION('center_axis',(-0.49999999999984,-0.49999999999984,-0.707106781186774)) ;
#4964 = DIRECTION('ref_axis',(-0.707106781186547,0.707106781186548,-3.33066907361881E-16)) ;
#4965 = DIRECTION('',(0.49999999999984,0.49999999999984,-0.707106781186774)) ;
#4966 = DIRECTION('center_axis',(-1.18423789293E-14,-8.881784197E-15,-1.)) ;
#4967 = DIRECTION('ref_axis',(0.587785252292138,0.809016994375191,-1.41462900424437E-14)) ;
#4968 = DIRECTION('',(0.707106781186547,5.11457513742672E-8,-0.707106781186547)) ;
#4969 = DIRECTION('center_axis',(-0.707106781186548,0.,-0.707106781186548)) ;
#4970 = DIRECTION('ref_axis',(0.,1.,0.)) ;
#4971 = DIRECTION('center_axis',(-0.707106781186548,0.,0.707106781186548)) ;
#4972 = DIRECTION('ref_axis',(0.,1.,0.)) ;
#4973 = DIRECTION('axis',(0.,0.,1.)) ;
#4974 = DIRECTION('refdir',(1.,0.,0.)) ;
#4975 = DIRECTION('center_axis',(5.3290705182E-15,-7.9936057773E-15,-1.)) ;
#4976 = DIRECTION('ref_axis',(1.38777878078155E-16,-1.,7.9936057773E-15)) ;
#4977 = DIRECTION('center_axis',(2.11939249808E-15,3.56296341164E-15,1.)) ;
#4978 = DIRECTION('ref_axis',(-1.,5.07218842173629E-46,2.11939249808E-15)) ;
#4979 = DIRECTION('center_axis',(2.11939249808E-15,3.56296341164E-15,1.)) ;
#4980 = DIRECTION('ref_axis',(-1.,5.07218842173629E-46,2.11939249808E-15)) ;
#4981 = DIRECTION('center_axis',(0.,0.,1.)) ;
#4982 = DIRECTION('ref_axis',(-0.997855551910869,-0.0654545454544914,0.)) ;
#4983 = DIRECTION('',(0.,0.,1.)) ;
#4984 = DIRECTION('center_axis',(0.,0.,1.)) ;
#4985 = DIRECTION('ref_axis',(-1.,0.,0.)) ;
#4986 = DIRECTION('',(0.,0.,1.)) ;
#4987 = DIRECTION('center_axis',(5.3290705182E-15,-7.9936057773E-15,1.)) ;
#4988 = DIRECTION('ref_axis',(-3.46944695195351E-16,-1.,-7.9936057773E-15)) ;
#4989 = DIRECTION('center_axis',(-2.11939249808E-15,-3.56296341164E-15,1.)) ;
#4990 = DIRECTION('ref_axis',(-1.,5.07218842173629E-46,-2.11939249808E-15)) ;
#4991 = DIRECTION('center_axis',(0.,0.,1.)) ;
#4992 = DIRECTION('ref_axis',(1.,0.,0.)) ;
#4993 = DIRECTION('',(1.,0.,0.)) ;
#4994 = DIRECTION('',(-1.,0.,0.)) ;
#4995 = DIRECTION('',(0.,1.,0.)) ;
#4996 = DIRECTION('center_axis',(0.,0.,1.)) ;
#4997 = DIRECTION('ref_axis',(-1.,0.,0.)) ;
#4998 = DIRECTION('',(-1.,0.,0.)) ;
#4999 = DIRECTION('center_axis',(0.,0.,1.)) ;
#5000 = DIRECTION('ref_axis',(-1.,0.,0.)) ;
#5001 = DIRECTION('',(-0.707106781186548,0.707106781186548,0.)) ;
#5002 = DIRECTION('center_axis',(0.,0.,1.)) ;
#5003 = DIRECTION('ref_axis',(-1.,0.,0.)) ;
#5004 = DIRECTION('',(-1.,0.,0.)) ;
#5005 = DIRECTION('center_axis',(0.,0.,1.)) ;
#5006 = DIRECTION('ref_axis',(-1.,0.,0.)) ;
#5007 = DIRECTION('',(0.707106781186548,0.707106781186548,0.)) ;
#5008 = DIRECTION('center_axis',(0.,0.,1.)) ;
#5009 = DIRECTION('ref_axis',(-1.,0.,0.)) ;
#5010 = DIRECTION('',(-1.,0.,0.)) ;
#5011 = DIRECTION('center_axis',(0.,0.,1.)) ;
#5012 = DIRECTION('ref_axis',(-1.,0.,0.)) ;
#5013 = DIRECTION('',(0.,1.,0.)) ;
#5014 = DIRECTION('center_axis',(0.,0.,-1.)) ;
#5015 = DIRECTION('ref_axis',(-0.951056516295124,0.30901699437504,0.)) ;
#5016 = DIRECTION('',(-0.707106781186548,4.18691322315732E-15,-0.707106781186548)) ;
#5017 = DIRECTION('center_axis',(0.,0.,1.)) ;
#5018 = DIRECTION('ref_axis',(-1.,0.,0.)) ;
#5019 = DIRECTION('',(0.,-0.707106781186548,-0.707106781186548)) ;
#5020 = DIRECTION('center_axis',(0.,0.707106781186548,-0.707106781186548)) ;
#5021 = DIRECTION('ref_axis',(-1.,0.,0.)) ;
#5022 = DIRECTION('',(-1.,0.,0.)) ;
#5023 = DIRECTION('',(0.,0.707106781186548,0.707106781186548)) ;
#5024 = DIRECTION('center_axis',(0.,-1.18423789293E-14,1.)) ;
#5025 = DIRECTION('ref_axis',(0.968449269396153,0.249210779474039,2.95124848379779E-15)) ;
#5026 = DIRECTION('center_axis',(2.85813443795E-15,-1.11068959943E-14,1.)) ;
#5027 = DIRECTION('ref_axis',(-1.,1.53049221729886E-46,2.85813443795E-15)) ;
#5028 = DIRECTION('',(0.49999999999984,0.49999999999984,0.707106781186774)) ;
#5029 = DIRECTION('center_axis',(0.49999999999984,0.49999999999984,-0.707106781186774)) ;
#5030 = DIRECTION('ref_axis',(-0.707106781186547,0.707106781186548,3.33066907361881E-16)) ;
#5031 = DIRECTION('',(-0.707106781186548,0.707106781186548,0.)) ;
#5032 = DIRECTION('',(0.49999999999984,0.49999999999984,0.707106781186774)) ;
#5033 = DIRECTION('center_axis',(0.,0.,-1.)) ;
#5034 = DIRECTION('ref_axis',(-0.770879376792195,-0.63698115077016,0.)) ;
#5035 = DIRECTION('center_axis',(0.,0.,1.)) ;
#5036 = DIRECTION('ref_axis',(-1.,0.,0.)) ;
#5037 = DIRECTION('',(0.,-0.707106781186548,-0.707106781186548)) ;
#5038 = DIRECTION('center_axis',(0.,0.707106781186548,-0.707106781186548)) ;
#5039 = DIRECTION('ref_axis',(-1.,0.,0.)) ;
#5040 = DIRECTION('',(-1.,0.,0.)) ;
#5041 = DIRECTION('',(0.,0.707106781186548,0.707106781186548)) ;
#5042 = DIRECTION('center_axis',(2.96059473233E-15,-1.18423789293E-14,-1.)) ;
#5043 = DIRECTION('ref_axis',(-0.839857192231928,-0.542807421334954,3.94165438985342E-15)) ;
#5044 = DIRECTION('center_axis',(-6.27102152096E-15,9.70281967417E-15,1.)) ;
#5045 = DIRECTION('ref_axis',(-1.,-4.77240444652696E-45,-6.27102152096E-15)) ;
#5046 = DIRECTION('',(0.49999999999984,-0.49999999999984,-0.707106781186774)) ;
#5047 = DIRECTION('center_axis',(0.49999999999984,-0.49999999999984,0.707106781186774)) ;
#5048 = DIRECTION('ref_axis',(0.707106781186547,0.707106781186548,3.33066907361881E-16)) ;
#5049 = DIRECTION('',(0.707106781186548,0.707106781186548,0.)) ;
#5050 = DIRECTION('',(-0.49999999999984,0.49999999999984,0.707106781186774)) ;
#5051 = DIRECTION('center_axis',(-5.92118946467E-15,5.92118946467E-15,1.)) ;
#5052 = DIRECTION('ref_axis',(0.097072775000982,0.995277286163815,-5.31843908861643E-15)) ;
#5053 = DIRECTION('center_axis',(-6.43746510567E-15,6.27867841924E-16,1.)) ;
#5054 = DIRECTION('ref_axis',(-1.,-2.64294780005913E-47,-6.43746510567E-15)) ;
#5055 = DIRECTION('',(0.,0.707106781186548,0.707106781186548)) ;
#5056 = DIRECTION('center_axis',(0.,0.707106781186548,-0.707106781186548)) ;
#5057 = DIRECTION('ref_axis',(-1.,0.,0.)) ;
#5058 = DIRECTION('',(-1.,0.,0.)) ;
#5059 = DIRECTION('',(0.,0.707106781186548,0.707106781186548)) ;
#5060 = DIRECTION('center_axis',(0.,0.,-1.)) ;
#5061 = DIRECTION('ref_axis',(0.707106799571885,-0.70710676280121,0.)) ;
#5062 = DIRECTION('center_axis',(0.,0.,1.)) ;
#5063 = DIRECTION('ref_axis',(-1.,0.,0.)) ;
#5064 = DIRECTION('',(0.707106781186548,-4.18691322315732E-15,-0.707106781186548)) ;
#5065 = DIRECTION('center_axis',(0.707106781186548,0.,0.707106781186548)) ;
#5066 = DIRECTION('ref_axis',(0.,1.,0.)) ;
#5067 = DIRECTION('',(0.,1.,0.)) ;
#5068 = DIRECTION('',(-0.707106781186548,0.,0.707106781186548)) ;
#5069 = DIRECTION('center_axis',(0.707106781186548,0.,-0.707106781186548)) ;
#5070 = DIRECTION('ref_axis',(0.,1.,0.)) ;
#5071 = DIRECTION('',(0.707106781186548,0.,0.707106781186548)) ;
#5072 = DIRECTION('',(0.,1.,0.)) ;
#5073 = DIRECTION('center_axis',(0.,0.,1.)) ;
#5074 = DIRECTION('ref_axis',(1.,0.,0.)) ;
#5075 = DIRECTION('',(0.,1.,0.)) ;
#5076 = DIRECTION('center_axis',(0.,0.,1.)) ;
#5077 = DIRECTION('ref_axis',(-1.,0.,0.)) ;
#5078 = DIRECTION('',(-1.,0.,0.)) ;
#5079 = DIRECTION('center_axis',(0.,0.,1.)) ;
#5080 = DIRECTION('ref_axis',(-1.,0.,0.)) ;
#5081 = DIRECTION('',(0.707106781186548,0.707106781186548,0.)) ;
#5082 = DIRECTION('center_axis',(0.,0.,1.)) ;
#5083 = DIRECTION('ref_axis',(-1.,0.,0.)) ;
#5084 = DIRECTION('',(-1.,0.,0.)) ;
#5085 = DIRECTION('center_axis',(0.,0.,1.)) ;
#5086 = DIRECTION('ref_axis',(-1.,0.,0.)) ;
#5087 = DIRECTION('',(-0.707106781186548,0.707106781186548,0.)) ;
#5088 = DIRECTION('center_axis',(0.,0.,1.)) ;
#5089 = DIRECTION('ref_axis',(-1.,0.,0.)) ;
#5090 = DIRECTION('',(-1.,0.,0.)) ;
#5091 = DIRECTION('center_axis',(0.,0.,1.)) ;
#5092 = DIRECTION('ref_axis',(-1.,0.,0.)) ;
#5093 = DIRECTION('',(0.,1.,0.)) ;
#5094 = DIRECTION('',(-1.,0.,0.)) ;
#5095 = DIRECTION('',(1.,0.,0.)) ;
#5096 = DIRECTION('center_axis',(0.,0.,1.)) ;
#5097 = DIRECTION('ref_axis',(0.,1.,0.)) ;
#5098 = DIRECTION('center_axis',(0.,0.,1.)) ;
#5099 = DIRECTION('ref_axis',(-1.,0.,0.)) ;
#5100 = DIRECTION('',(0.,0.,1.)) ;
#5101 = DIRECTION('',(0.,0.,1.)) ;
#5102 = DIRECTION('center_axis',(0.,0.,1.)) ;
#5103 = DIRECTION('ref_axis',(-0.707106781186548,-0.707106781186548,0.)) ;
#5104 = DIRECTION('',(0.,0.,1.)) ;
#5105 = DIRECTION('',(0.,0.,1.)) ;
#5106 = DIRECTION('center_axis',(0.,0.,1.)) ;
#5107 = DIRECTION('ref_axis',(-1.,0.,0.)) ;
#5108 = DIRECTION('center_axis',(-0.707106781186548,-0.707106781186548,0.)) ;
#5109 = DIRECTION('ref_axis',(0.707106781186548,-0.707106781186548,0.)) ;
#5110 = DIRECTION('',(0.,0.,1.)) ;
#5111 = DIRECTION('',(-0.707106781186548,0.707106781186548,0.)) ;
#5112 = DIRECTION('center_axis',(-0.707106781186548,0.707106781186548,0.)) ;
#5113 = DIRECTION('ref_axis',(-0.707106781186548,-0.707106781186548,0.)) ;
#5114 = DIRECTION('',(0.707106781186548,0.707106781186548,0.)) ;
#5115 = DIRECTION('',(0.,0.,1.)) ;
#5116 = DIRECTION('center_axis',(0.,0.,1.)) ;
#5117 = DIRECTION('ref_axis',(1.11022302463E-16,-1.,0.)) ;
#5118 = DIRECTION('',(0.,0.,1.)) ;
#5119 = DIRECTION('center_axis',(0.,0.,1.)) ;
#5120 = DIRECTION('ref_axis',(-1.,0.,0.)) ;
#5121 = DIRECTION('center_axis',(0.,-1.,0.)) ;
#5122 = DIRECTION('ref_axis',(1.,0.,0.)) ;
#5123 = DIRECTION('',(-1.,0.,0.)) ;
#5124 = DIRECTION('center_axis',(0.,0.,1.)) ;
#5125 = DIRECTION('ref_axis',(0.707106781186548,0.707106781186548,0.)) ;
#5126 = DIRECTION('center_axis',(0.,0.,1.)) ;
#5127 = DIRECTION('ref_axis',(-1.,0.,0.)) ;
#5128 = DIRECTION('',(0.,0.,1.)) ;
#5129 = DIRECTION('center_axis',(0.,1.,0.)) ;
#5130 = DIRECTION('ref_axis',(-1.,0.,0.)) ;
#5131 = DIRECTION('',(0.,0.,1.)) ;
#5132 = DIRECTION('',(-0.707106781186548,0.,-0.707106781186548)) ;
#5133 = DIRECTION('center_axis',(0.,1.,0.)) ;
#5134 = DIRECTION('ref_axis',(0.,0.,-1.)) ;
#5135 = DIRECTION('center_axis',(0.,1.,0.)) ;
#5136 = DIRECTION('ref_axis',(0.,0.,-1.)) ;
#5137 = DIRECTION('center_axis',(0.,1.,0.)) ;
#5138 = DIRECTION('ref_axis',(-1.,0.,0.)) ;
#5139 = DIRECTION('',(0.,0.,1.)) ;
#5140 = DIRECTION('',(0.707106781186548,0.,-0.707106781186548)) ;
#5141 = DIRECTION('center_axis',(0.,1.,0.)) ;
#5142 = DIRECTION('ref_axis',(0.,0.,-1.)) ;
#5143 = DIRECTION('center_axis',(0.,1.,0.)) ;
#5144 = DIRECTION('ref_axis',(0.,0.,-1.)) ;
#5145 = DIRECTION('center_axis',(-1.,0.,0.)) ;
#5146 = DIRECTION('ref_axis',(0.,-1.,0.)) ;
#5147 = DIRECTION('',(0.,1.,0.)) ;
#5148 = DIRECTION('',(0.,0.,1.)) ;
#5149 = DIRECTION('center_axis',(0.,0.,1.)) ;
#5150 = DIRECTION('ref_axis',(1.13626224362E-14,-1.,0.)) ;
#5151 = DIRECTION('',(0.,0.,1.)) ;
#5152 = DIRECTION('center_axis',(0.,0.,1.)) ;
#5153 = DIRECTION('ref_axis',(-1.,0.,0.)) ;
#5154 = DIRECTION('center_axis',(-1.,0.,0.)) ;
#5155 = DIRECTION('ref_axis',(0.,-1.,0.)) ;
#5156 = DIRECTION('',(0.,0.,1.)) ;
#5157 = DIRECTION('',(0.,1.,0.)) ;
#5158 = DIRECTION('center_axis',(0.,0.,1.)) ;
#5159 = DIRECTION('ref_axis',(-1.,1.83697019872E-16,0.)) ;
#5160 = DIRECTION('',(0.,0.,1.)) ;
#5161 = DIRECTION('center_axis',(0.,0.,1.)) ;
#5162 = DIRECTION('ref_axis',(-1.,0.,0.)) ;
#5163 = DIRECTION('center_axis',(0.,0.,1.)) ;
#5164 = DIRECTION('ref_axis',(-0.951056516295124,0.30901699437504,0.)) ;
#5165 = DIRECTION('',(-0.707106780871626,2.11010493413889E-5,0.707106781186626)) ;
#5166 = DIRECTION('',(0.,-0.707106781186548,0.707106781186548)) ;
#5167 = DIRECTION('center_axis',(0.,-0.707106781186548,-0.707106781186548)) ;
#5168 = DIRECTION('ref_axis',(-1.,0.,0.)) ;
#5169 = DIRECTION('',(0.,0.707106781186548,-0.707106781186548)) ;
#5170 = DIRECTION('',(-1.,0.,0.)) ;
#5171 = DIRECTION('center_axis',(0.,-1.18423789293E-14,-1.)) ;
#5172 = DIRECTION('ref_axis',(0.968449269396153,0.249210779474039,-2.95124848379779E-15)) ;
#5173 = DIRECTION('',(0.49999999999984,0.49999999999984,-0.707106781186774)) ;
#5174 = DIRECTION('center_axis',(-0.49999999999984,-0.49999999999984,-0.707106781186774)) ;
#5175 = DIRECTION('ref_axis',(-0.707106781186547,0.707106781186548,-3.33066907361881E-16)) ;
#5176 = DIRECTION('',(0.49999999999984,0.49999999999984,-0.707106781186774)) ;
#5177 = DIRECTION('center_axis',(0.,0.,1.)) ;
#5178 = DIRECTION('ref_axis',(-0.770879376792195,-0.63698115077016,0.)) ;
#5179 = DIRECTION('',(0.,-0.707106781186548,0.707106781186548)) ;
#5180 = DIRECTION('center_axis',(0.,-0.707106781186548,-0.707106781186548)) ;
#5181 = DIRECTION('ref_axis',(-1.,0.,0.)) ;
#5182 = DIRECTION('',(0.,0.707106781186548,-0.707106781186548)) ;
#5183 = DIRECTION('center_axis',(2.96059473233E-15,-1.18423789293E-14,1.)) ;
#5184 = DIRECTION('ref_axis',(-0.839857192231928,-0.542807421334954,-3.94165438985342E-15)) ;
#5185 = DIRECTION('',(0.50000001947084,-0.49999998052884,0.707106781186774)) ;
#5186 = DIRECTION('center_axis',(-0.49999999999984,0.49999999999984,0.707106781186774)) ;
#5187 = DIRECTION('ref_axis',(0.707106781186547,0.707106781186548,-3.33066907361881E-16)) ;
#5188 = DIRECTION('',(-0.49999999999984,0.49999999999984,-0.707106781186774)) ;
#5189 = DIRECTION('center_axis',(-5.92118946467E-15,5.92118946467E-15,-1.)) ;
#5190 = DIRECTION('ref_axis',(0.097072775000982,0.995277286163815,5.31843908861643E-15)) ;
#5191 = DIRECTION('',(-4.28670243814725E-8,0.707106781186547,-0.707106781186547)) ;
#5192 = DIRECTION('center_axis',(0.,-0.707106781186548,-0.707106781186548)) ;
#5193 = DIRECTION('ref_axis',(-1.,0.,0.)) ;
#5194 = DIRECTION('',(0.,0.707106781186548,-0.707106781186548)) ;
#5195 = DIRECTION('',(-1.,0.,0.)) ;
#5196 = DIRECTION('center_axis',(0.,0.,1.)) ;
#5197 = DIRECTION('ref_axis',(0.707118857908102,-0.70709470425873,0.)) ;
#5198 = DIRECTION('',(0.707106780773791,2.41533135191928E-5,0.707106781186791)) ;
#5199 = DIRECTION('center_axis',(-0.707106781186548,0.,0.707106781186548)) ;
#5200 = DIRECTION('ref_axis',(0.,1.,0.)) ;
#5201 = DIRECTION('center_axis',(-0.707106781186548,0.,-0.707106781186548)) ;
#5202 = DIRECTION('ref_axis',(0.,1.,0.)) ;
#5203 = DIRECTION('center_axis',(0.,1.,0.)) ;
#5204 = DIRECTION('ref_axis',(0.877582561890372,0.,-0.479425538604204)) ;
#5205 = DIRECTION('center_axis',(0.,1.,0.)) ;
#5206 = DIRECTION('ref_axis',(0.,0.,-1.)) ;
#5207 = DIRECTION('',(0.,1.,0.)) ;
#5208 = DIRECTION('center_axis',(0.,1.,0.)) ;
#5209 = DIRECTION('ref_axis',(0.,0.,-1.)) ;
#5210 = DIRECTION('center_axis',(1.42108547152E-14,-1.,3.16191517413E-13)) ;
#5211 = DIRECTION('ref_axis',(-0.811184158891276,1.73378264946965E-13,0.584790783412199)) ;
#5212 = DIRECTION('',(0.573593819543454,-0.70710678118628,-0.413509528526164)) ;
#5213 = DIRECTION('center_axis',(1.54852556736E-13,-1.,2.14801506028E-13)) ;
#5214 = DIRECTION('ref_axis',(4.47622740477785E-43,2.14801506028E-13,1.)) ;
#5215 = DIRECTION('center_axis',(0.,1.,0.)) ;
#5216 = DIRECTION('ref_axis',(0.877582561890372,0.,-0.479425538604204)) ;
#5217 = DIRECTION('center_axis',(0.,1.,0.)) ;
#5218 = DIRECTION('ref_axis',(0.,0.,-1.)) ;
#5219 = DIRECTION('',(0.,1.,0.)) ;
#5220 = DIRECTION('center_axis',(0.,1.,0.)) ;
#5221 = DIRECTION('ref_axis',(0.,0.,-1.)) ;
#5222 = DIRECTION('center_axis',(0.,-1.,0.)) ;
#5223 = DIRECTION('ref_axis',(1.,0.,0.)) ;
#5224 = DIRECTION('center_axis',(0.,-1.,0.)) ;
#5225 = DIRECTION('ref_axis',(0.,0.,1.)) ;
#5226 = DIRECTION('center_axis',(2.84217094304E-14,-1.,3.19744231092E-13)) ;
#5227 = DIRECTION('ref_axis',(-0.811184158893383,1.63928238932276E-13,0.584790783409276)) ;
#5228 = DIRECTION('',(0.573593819544954,-0.707106781186273,-0.413509528524095)) ;
#5229 = DIRECTION('center_axis',(0.,1.,0.)) ;
#5230 = DIRECTION('ref_axis',(0.877582561890372,0.,-0.479425538604204)) ;
#5231 = DIRECTION('center_axis',(0.,1.,0.)) ;
#5232 = DIRECTION('ref_axis',(0.,0.,-1.)) ;
#5233 = DIRECTION('',(0.,1.,0.)) ;
#5234 = DIRECTION('center_axis',(0.,1.,0.)) ;
#5235 = DIRECTION('ref_axis',(0.,0.,-1.)) ;
#5236 = DIRECTION('center_axis',(2.84217094304E-14,-1.,3.23296944771E-13)) ;
#5237 = DIRECTION('ref_axis',(-0.811184158891618,1.66005833148689E-13,0.584790783411725)) ;
#5238 = DIRECTION('',(0.573593819543705,-0.707106781186275,-0.413509528525824)) ;
#5239 = DIRECTION('center_axis',(1.63083011564E-13,-1.,2.26218263553E-13)) ;
#5240 = DIRECTION('ref_axis',(1.41626863241979E-42,2.26218263553E-13,1.)) ;
#5241 = DIRECTION('center_axis',(0.,1.,0.)) ;
#5242 = DIRECTION('ref_axis',(0.877582561890372,0.,-0.479425538604204)) ;
#5243 = DIRECTION('center_axis',(0.,1.,0.)) ;
#5244 = DIRECTION('ref_axis',(0.,0.,-1.)) ;
#5245 = DIRECTION('',(0.,1.,0.)) ;
#5246 = DIRECTION('center_axis',(0.,1.,0.)) ;
#5247 = DIRECTION('ref_axis',(0.,0.,-1.)) ;
#5248 = DIRECTION('center_axis',(0.,-1.,0.)) ;
#5249 = DIRECTION('ref_axis',(1.,0.,0.)) ;
#5250 = DIRECTION('center_axis',(0.,-1.,0.)) ;
#5251 = DIRECTION('ref_axis',(0.,0.,1.)) ;
#5252 = DIRECTION('center_axis',(4.26325641456E-14,-1.,3.23296944771E-13)) ;
#5253 = DIRECTION('ref_axis',(-0.811184158884955,1.54478212922681E-13,0.584790783420967)) ;
#5254 = DIRECTION('',(0.573593819539004,-0.707106781186267,-0.413509528532359)) ;
#5255 = DIRECTION('axis',(0.,0.,1.)) ;
#5256 = DIRECTION('refdir',(1.,0.,0.)) ;
#5257 = DIRECTION('center_axis',(0.,-1.,0.)) ;
#5258 = DIRECTION('ref_axis',(1.,0.,0.)) ;
#5259 = DIRECTION('center_axis',(0.,-1.,0.)) ;
#5260 = DIRECTION('ref_axis',(0.,0.,1.)) ;
#5261 = DIRECTION('',(0.,1.,0.)) ;
#5262 = DIRECTION('center_axis',(0.,-1.,0.)) ;
#5263 = DIRECTION('ref_axis',(0.,0.,1.)) ;
#5264 = DIRECTION('center_axis',(0.,-1.,0.)) ;
#5265 = DIRECTION('ref_axis',(1.,0.,0.)) ;
#5266 = DIRECTION('center_axis',(0.,-1.,0.)) ;
#5267 = DIRECTION('ref_axis',(0.,0.,1.)) ;
#5268 = DIRECTION('',(0.,-1.,0.)) ;
#5269 = DIRECTION('center_axis',(0.,-1.,0.)) ;
#5270 = DIRECTION('ref_axis',(0.,0.,1.)) ;
#5271 = DIRECTION('center_axis',(0.,-1.,0.)) ;
#5272 = DIRECTION('ref_axis',(1.,0.,0.)) ;
#5273 = DIRECTION('center_axis',(0.,-1.,0.)) ;
#5274 = DIRECTION('ref_axis',(1.,0.,0.)) ;
#5275 = DIRECTION('axis',(0.,0.,1.)) ;
#5276 = DIRECTION('refdir',(1.,0.,0.)) ;
#5277 = DIRECTION('center_axis',(0.,-1.,0.)) ;
#5278 = DIRECTION('ref_axis',(1.,0.,0.)) ;
#5279 = DIRECTION('center_axis',(0.,-1.,0.)) ;
#5280 = DIRECTION('ref_axis',(0.,0.,1.)) ;
#5281 = DIRECTION('',(0.,1.,0.)) ;
#5282 = DIRECTION('center_axis',(0.,-1.,0.)) ;
#5283 = DIRECTION('ref_axis',(0.,0.,1.)) ;
#5284 = DIRECTION('center_axis',(0.,-1.,0.)) ;
#5285 = DIRECTION('ref_axis',(1.,0.,0.)) ;
#5286 = DIRECTION('center_axis',(0.,-1.,0.)) ;
#5287 = DIRECTION('ref_axis',(0.,0.,1.)) ;
#5288 = DIRECTION('',(0.,-1.,0.)) ;
#5289 = DIRECTION('center_axis',(0.,-1.,0.)) ;
#5290 = DIRECTION('ref_axis',(0.,0.,1.)) ;
#5291 = DIRECTION('center_axis',(0.,-1.,0.)) ;
#5292 = DIRECTION('ref_axis',(1.,0.,0.)) ;
#5293 = DIRECTION('center_axis',(0.,-1.,0.)) ;
#5294 = DIRECTION('ref_axis',(1.,0.,0.)) ;
#5295 = DIRECTION('axis',(0.,0.,1.)) ;
#5296 = DIRECTION('refdir',(1.,0.,0.)) ;
#5297 = DIRECTION('center_axis',(0.,-1.,0.)) ;
#5298 = DIRECTION('ref_axis',(1.,0.,0.)) ;
#5299 = DIRECTION('center_axis',(0.,-1.,0.)) ;
#5300 = DIRECTION('ref_axis',(0.,0.,1.)) ;
#5301 = DIRECTION('',(0.,1.,0.)) ;
#5302 = DIRECTION('center_axis',(0.,-1.,0.)) ;
#5303 = DIRECTION('ref_axis',(0.,0.,1.)) ;
#5304 = DIRECTION('center_axis',(0.,-1.,0.)) ;
#5305 = DIRECTION('ref_axis',(1.,0.,0.)) ;
#5306 = DIRECTION('center_axis',(0.,-1.,0.)) ;
#5307 = DIRECTION('ref_axis',(0.,0.,1.)) ;
#5308 = DIRECTION('',(0.,-1.,0.)) ;
#5309 = DIRECTION('center_axis',(0.,-1.,0.)) ;
#5310 = DIRECTION('ref_axis',(0.,0.,1.)) ;
#5311 = DIRECTION('center_axis',(0.,-1.,0.)) ;
#5312 = DIRECTION('ref_axis',(1.,0.,0.)) ;
#5313 = DIRECTION('center_axis',(0.,-1.,0.)) ;
#5314 = DIRECTION('ref_axis',(1.,0.,0.)) ;
#5315 = DIRECTION('axis',(0.,0.,1.)) ;
#5316 = DIRECTION('refdir',(1.,0.,0.)) ;
#5317 = DIRECTION('center_axis',(0.,-1.,0.)) ;
#5318 = DIRECTION('ref_axis',(1.,0.,0.)) ;
#5319 = DIRECTION('center_axis',(0.,-1.,0.)) ;
#5320 = DIRECTION('ref_axis',(0.,0.,1.)) ;
#5321 = DIRECTION('',(0.,1.,0.)) ;
#5322 = DIRECTION('center_axis',(0.,-1.,0.)) ;
#5323 = DIRECTION('ref_axis',(0.,0.,1.)) ;
#5324 = DIRECTION('center_axis',(0.,-1.,0.)) ;
#5325 = DIRECTION('ref_axis',(1.,0.,0.)) ;
#5326 = DIRECTION('center_axis',(0.,-1.,0.)) ;
#5327 = DIRECTION('ref_axis',(0.,0.,1.)) ;
#5328 = DIRECTION('',(0.,-1.,0.)) ;
#5329 = DIRECTION('center_axis',(0.,-1.,0.)) ;
#5330 = DIRECTION('ref_axis',(0.,0.,1.)) ;
#5331 = DIRECTION('center_axis',(0.,-1.,0.)) ;
#5332 = DIRECTION('ref_axis',(1.,0.,0.)) ;
#5333 = DIRECTION('center_axis',(0.,-1.,0.)) ;
#5334 = DIRECTION('ref_axis',(1.,0.,0.)) ;
#5335 = DIRECTION('axis',(0.,0.,1.)) ;
#5336 = DIRECTION('refdir',(1.,0.,0.)) ;
#5337 = DIRECTION('center_axis',(1.,0.,-1.53837014911E-16)) ;
#5338 = DIRECTION('ref_axis',(-1.53837014911E-16,0.,-1.)) ;
#5339 = DIRECTION('',(0.,1.,0.)) ;
#5340 = DIRECTION('',(0.,0.,-1.)) ;
#5341 = DIRECTION('',(0.,1.,0.)) ;
#5342 = DIRECTION('',(0.,0.,-1.)) ;
#5343 = DIRECTION('center_axis',(0.50000000000019,0.,-0.866025403784329)) ;
#5344 = DIRECTION('ref_axis',(-0.866025403784329,0.,-0.50000000000019)) ;
#5345 = DIRECTION('',(0.,1.,0.)) ;
#5346 = DIRECTION('',(-0.866025403784329,0.,-0.50000000000019)) ;
#5347 = DIRECTION('',(-0.866025403784329,0.,-0.50000000000019)) ;
#5348 = DIRECTION('center_axis',(0.50000000000019,0.,0.866025403784329)) ;
#5349 = DIRECTION('ref_axis',(0.866025403784329,0.,-0.50000000000019)) ;
#5350 = DIRECTION('',(0.866025403784329,0.,-0.50000000000019)) ;
#5351 = DIRECTION('',(0.,1.,0.)) ;
#5352 = DIRECTION('',(0.866025403784329,0.,-0.50000000000019)) ;
#5353 = DIRECTION('center_axis',(0.,-1.,0.)) ;
#5354 = DIRECTION('ref_axis',(1.,0.,0.)) ;
#5355 = DIRECTION('',(0.866025403784329,0.,0.50000000000019)) ;
#5356 = DIRECTION('',(0.,0.,1.)) ;
#5357 = DIRECTION('',(-0.866025403784329,0.,0.50000000000019)) ;
#5358 = DIRECTION('center_axis',(-0.50000000000019,0.,-0.866025403784329)) ;
#5359 = DIRECTION('ref_axis',(-0.866025403784329,0.,0.50000000000019)) ;
#5360 = DIRECTION('',(0.,1.,0.)) ;
#5361 = DIRECTION('',(-0.866025403784329,0.,0.50000000000019)) ;
#5362 = DIRECTION('center_axis',(-0.50000000000019,0.,0.866025403784329)) ;
#5363 = DIRECTION('ref_axis',(0.866025403784329,0.,0.50000000000019)) ;
#5364 = DIRECTION('',(0.866025403784329,0.,0.50000000000019)) ;
#5365 = DIRECTION('',(0.,1.,0.)) ;
#5366 = DIRECTION('center_axis',(-1.,0.,0.)) ;
#5367 = DIRECTION('ref_axis',(0.,0.,1.)) ;
#5368 = DIRECTION('',(0.,0.,1.)) ;
#5369 = DIRECTION('center_axis',(0.,-1.,0.)) ;
#5370 = DIRECTION('ref_axis',(-1.,0.,0.)) ;
#5371 = DIRECTION('center_axis',(0.,-1.,0.)) ;
#5372 = DIRECTION('ref_axis',(0.,0.,1.)) ;
#5373 = DIRECTION('center_axis',(0.,-1.,0.)) ;
#5374 = DIRECTION('ref_axis',(-1.,0.,0.)) ;
#5375 = DIRECTION('center_axis',(0.,-1.,0.)) ;
#5376 = DIRECTION('ref_axis',(0.,0.,1.)) ;
#5377 = DIRECTION('center_axis',(0.,-1.,0.)) ;
#5378 = DIRECTION('ref_axis',(0.,0.,1.)) ;
#5379 = DIRECTION('center_axis',(0.,-1.,0.)) ;
#5380 = DIRECTION('ref_axis',(-1.,0.,0.)) ;
#5381 = DIRECTION('center_axis',(0.,-1.,0.)) ;
#5382 = DIRECTION('ref_axis',(0.,0.,1.)) ;
#5383 = DIRECTION('center_axis',(0.,-1.,0.)) ;
#5384 = DIRECTION('ref_axis',(0.479425538604205,0.,-0.877582561890372)) ;
#5385 = DIRECTION('center_axis',(-0.877582561890372,0.,-0.479425538604205)) ;
#5386 = DIRECTION('ref_axis',(-0.479425538604205,0.,0.877582561890372)) ;
#5387 = DIRECTION('center_axis',(0.,-1.,0.)) ;
#5388 = DIRECTION('ref_axis',(0.,0.,1.)) ;
#5389 = DIRECTION('center_axis',(0.,-1.,0.)) ;
#5390 = DIRECTION('ref_axis',(0.479425538604204,0.,-0.877582561890372)) ;
#5391 = DIRECTION('',(0.,1.,0.)) ;
#5392 = DIRECTION('center_axis',(0.,-1.,0.)) ;
#5393 = DIRECTION('ref_axis',(0.479425538604204,0.,-0.877582561890372)) ;
#5394 = DIRECTION('center_axis',(0.877582561890372,0.,0.479425538604204)) ;
#5395 = DIRECTION('ref_axis',(-0.479425538604204,0.,0.877582561890372)) ;
#5396 = DIRECTION('center_axis',(0.,-1.,0.)) ;
#5397 = DIRECTION('ref_axis',(0.,0.,1.)) ;
#5398 = DIRECTION('center_axis',(0.,-1.,0.)) ;
#5399 = DIRECTION('ref_axis',(0.479425538604204,0.,-0.877582561890372)) ;
#5400 = DIRECTION('',(0.,1.,0.)) ;
#5401 = DIRECTION('center_axis',(0.,-1.,0.)) ;
#5402 = DIRECTION('ref_axis',(0.,0.,1.)) ;
#5403 = DIRECTION('center_axis',(0.,-1.,0.)) ;
#5404 = DIRECTION('ref_axis',(0.479425538604204,0.,-0.877582561890372)) ;
#5405 = DIRECTION('',(0.339005049420894,0.707106781186865,-0.620544580563467)) ;
#5406 = DIRECTION('axis',(0.,0.,1.)) ;
#5407 = DIRECTION('refdir',(1.,0.,0.)) ;
#5408 = DIRECTION('center_axis',(1.,0.,-1.53837014911E-16)) ;
#5409 = DIRECTION('ref_axis',(-1.53837014911E-16,0.,-1.)) ;
#5410 = DIRECTION('',(0.,1.,0.)) ;
#5411 = DIRECTION('',(0.,0.,-1.)) ;
#5412 = DIRECTION('',(0.,1.,0.)) ;
#5413 = DIRECTION('',(0.,0.,-1.)) ;
#5414 = DIRECTION('center_axis',(0.50000000000019,0.,-0.866025403784329)) ;
#5415 = DIRECTION('ref_axis',(-0.866025403784329,0.,-0.50000000000019)) ;
#5416 = DIRECTION('',(0.,1.,0.)) ;
#5417 = DIRECTION('',(-0.866025403784329,0.,-0.50000000000019)) ;
#5418 = DIRECTION('',(-0.866025403784329,0.,-0.50000000000019)) ;
#5419 = DIRECTION('center_axis',(0.50000000000019,0.,0.866025403784329)) ;
#5420 = DIRECTION('ref_axis',(0.866025403784329,0.,-0.50000000000019)) ;
#5421 = DIRECTION('',(0.866025403784329,0.,-0.50000000000019)) ;
#5422 = DIRECTION('',(0.,1.,0.)) ;
#5423 = DIRECTION('',(0.866025403784329,0.,-0.50000000000019)) ;
#5424 = DIRECTION('center_axis',(0.,-1.,0.)) ;
#5425 = DIRECTION('ref_axis',(1.,0.,0.)) ;
#5426 = DIRECTION('',(0.866025403784329,0.,0.50000000000019)) ;
#5427 = DIRECTION('',(0.,0.,1.)) ;
#5428 = DIRECTION('',(-0.866025403784329,0.,0.50000000000019)) ;
#5429 = DIRECTION('center_axis',(-0.50000000000019,0.,-0.866025403784329)) ;
#5430 = DIRECTION('ref_axis',(-0.866025403784329,0.,0.50000000000019)) ;
#5431 = DIRECTION('',(0.,1.,0.)) ;
#5432 = DIRECTION('',(-0.866025403784329,0.,0.50000000000019)) ;
#5433 = DIRECTION('center_axis',(-0.50000000000019,0.,0.866025403784329)) ;
#5434 = DIRECTION('ref_axis',(0.866025403784329,0.,0.50000000000019)) ;
#5435 = DIRECTION('',(0.866025403784329,0.,0.50000000000019)) ;
#5436 = DIRECTION('',(0.,1.,0.)) ;
#5437 = DIRECTION('center_axis',(-1.,0.,0.)) ;
#5438 = DIRECTION('ref_axis',(0.,0.,1.)) ;
#5439 = DIRECTION('',(0.,0.,1.)) ;
#5440 = DIRECTION('center_axis',(0.,-1.,0.)) ;
#5441 = DIRECTION('ref_axis',(-1.,0.,0.)) ;
#5442 = DIRECTION('center_axis',(0.,-1.,0.)) ;
#5443 = DIRECTION('ref_axis',(0.,0.,1.)) ;
#5444 = DIRECTION('center_axis',(0.,-1.,0.)) ;
#5445 = DIRECTION('ref_axis',(-1.,0.,0.)) ;
#5446 = DIRECTION('center_axis',(0.,-1.,0.)) ;
#5447 = DIRECTION('ref_axis',(0.,0.,1.)) ;
#5448 = DIRECTION('center_axis',(0.,-1.,0.)) ;
#5449 = DIRECTION('ref_axis',(0.,0.,1.)) ;
#5450 = DIRECTION('center_axis',(0.,-1.,0.)) ;
#5451 = DIRECTION('ref_axis',(-1.,0.,0.)) ;
#5452 = DIRECTION('center_axis',(0.,-1.,0.)) ;
#5453 = DIRECTION('ref_axis',(0.,0.,1.)) ;
#5454 = DIRECTION('center_axis',(0.,-1.,0.)) ;
#5455 = DIRECTION('ref_axis',(0.479425538604205,0.,-0.877582561890372)) ;
#5456 = DIRECTION('center_axis',(-0.877582561890372,0.,-0.479425538604205)) ;
#5457 = DIRECTION('ref_axis',(-0.479425538604205,0.,0.877582561890372)) ;
#5458 = DIRECTION('center_axis',(0.,-1.,0.)) ;
#5459 = DIRECTION('ref_axis',(0.,0.,1.)) ;
#5460 = DIRECTION('center_axis',(0.,-1.,0.)) ;
#5461 = DIRECTION('ref_axis',(0.479425538604204,0.,-0.877582561890372)) ;
#5462 = DIRECTION('',(0.,1.,0.)) ;
#5463 = DIRECTION('center_axis',(0.,-1.,0.)) ;
#5464 = DIRECTION('ref_axis',(0.479425538604204,0.,-0.877582561890372)) ;
#5465 = DIRECTION('center_axis',(0.877582561890372,0.,0.479425538604204)) ;
#5466 = DIRECTION('ref_axis',(-0.479425538604204,0.,0.877582561890372)) ;
#5467 = DIRECTION('center_axis',(0.,-1.,0.)) ;
#5468 = DIRECTION('ref_axis',(0.,0.,1.)) ;
#5469 = DIRECTION('center_axis',(0.,-1.,0.)) ;
#5470 = DIRECTION('ref_axis',(0.479425538604204,0.,-0.877582561890372)) ;
#5471 = DIRECTION('',(0.,1.,0.)) ;
#5472 = DIRECTION('center_axis',(0.,-1.,0.)) ;
#5473 = DIRECTION('ref_axis',(0.,0.,1.)) ;
#5474 = DIRECTION('center_axis',(0.,-1.,0.)) ;
#5475 = DIRECTION('ref_axis',(0.479425538604204,0.,-0.877582561890372)) ;
#5476 = DIRECTION('',(0.339005049420894,0.707106781186865,-0.620544580563467)) ;
#5477 = DIRECTION('axis',(0.,0.,1.)) ;
#5478 = DIRECTION('refdir',(1.,0.,0.)) ;
#5479 = DIRECTION('center_axis',(1.,0.,-1.53837014911E-16)) ;
#5480 = DIRECTION('ref_axis',(-1.53837014911E-16,0.,-1.)) ;
#5481 = DIRECTION('',(0.,1.,0.)) ;
#5482 = DIRECTION('',(0.,0.,-1.)) ;
#5483 = DIRECTION('',(0.,1.,0.)) ;
#5484 = DIRECTION('',(0.,0.,-1.)) ;
#5485 = DIRECTION('center_axis',(0.50000000000019,0.,-0.866025403784329)) ;
#5486 = DIRECTION('ref_axis',(-0.866025403784329,0.,-0.50000000000019)) ;
#5487 = DIRECTION('',(0.,1.,0.)) ;
#5488 = DIRECTION('',(-0.866025403784329,0.,-0.50000000000019)) ;
#5489 = DIRECTION('',(-0.866025403784329,0.,-0.50000000000019)) ;
#5490 = DIRECTION('center_axis',(0.50000000000019,0.,0.866025403784329)) ;
#5491 = DIRECTION('ref_axis',(0.866025403784329,0.,-0.50000000000019)) ;
#5492 = DIRECTION('',(0.866025403784329,0.,-0.50000000000019)) ;
#5493 = DIRECTION('',(0.,1.,0.)) ;
#5494 = DIRECTION('',(0.866025403784329,0.,-0.50000000000019)) ;
#5495 = DIRECTION('center_axis',(0.,-1.,0.)) ;
#5496 = DIRECTION('ref_axis',(1.,0.,0.)) ;
#5497 = DIRECTION('',(0.866025403784329,0.,0.50000000000019)) ;
#5498 = DIRECTION('',(0.,0.,1.)) ;
#5499 = DIRECTION('',(-0.866025403784329,0.,0.50000000000019)) ;
#5500 = DIRECTION('center_axis',(-0.50000000000019,0.,-0.866025403784329)) ;
#5501 = DIRECTION('ref_axis',(-0.866025403784329,0.,0.50000000000019)) ;
#5502 = DIRECTION('',(0.,1.,0.)) ;
#5503 = DIRECTION('',(-0.866025403784329,0.,0.50000000000019)) ;
#5504 = DIRECTION('center_axis',(-0.50000000000019,0.,0.866025403784329)) ;
#5505 = DIRECTION('ref_axis',(0.866025403784329,0.,0.50000000000019)) ;
#5506 = DIRECTION('',(0.866025403784329,0.,0.50000000000019)) ;
#5507 = DIRECTION('',(0.,1.,0.)) ;
#5508 = DIRECTION('center_axis',(-1.,0.,0.)) ;
#5509 = DIRECTION('ref_axis',(0.,0.,1.)) ;
#5510 = DIRECTION('',(0.,0.,1.)) ;
#5511 = DIRECTION('center_axis',(0.,-1.,0.)) ;
#5512 = DIRECTION('ref_axis',(-1.,0.,0.)) ;
#5513 = DIRECTION('center_axis',(0.,-1.,0.)) ;
#5514 = DIRECTION('ref_axis',(0.,0.,1.)) ;
#5515 = DIRECTION('center_axis',(0.,-1.,0.)) ;
#5516 = DIRECTION('ref_axis',(-1.,0.,0.)) ;
#5517 = DIRECTION('center_axis',(0.,-1.,0.)) ;
#5518 = DIRECTION('ref_axis',(0.,0.,1.)) ;
#5519 = DIRECTION('center_axis',(0.,-1.,0.)) ;
#5520 = DIRECTION('ref_axis',(0.,0.,1.)) ;
#5521 = DIRECTION('center_axis',(0.,-1.,0.)) ;
#5522 = DIRECTION('ref_axis',(-1.,0.,0.)) ;
#5523 = DIRECTION('center_axis',(0.,-1.,0.)) ;
#5524 = DIRECTION('ref_axis',(0.,0.,1.)) ;
#5525 = DIRECTION('center_axis',(0.,-1.,0.)) ;
#5526 = DIRECTION('ref_axis',(0.479425538604205,0.,-0.877582561890372)) ;
#5527 = DIRECTION('center_axis',(-0.877582561890372,0.,-0.479425538604205)) ;
#5528 = DIRECTION('ref_axis',(-0.479425538604205,0.,0.877582561890372)) ;
#5529 = DIRECTION('center_axis',(0.,-1.,0.)) ;
#5530 = DIRECTION('ref_axis',(0.,0.,1.)) ;
#5531 = DIRECTION('center_axis',(0.,-1.,0.)) ;
#5532 = DIRECTION('ref_axis',(0.479425538604204,0.,-0.877582561890372)) ;
#5533 = DIRECTION('',(0.,1.,0.)) ;
#5534 = DIRECTION('center_axis',(0.,-1.,0.)) ;
#5535 = DIRECTION('ref_axis',(0.479425538604204,0.,-0.877582561890372)) ;
#5536 = DIRECTION('center_axis',(0.877582561890372,0.,0.479425538604204)) ;
#5537 = DIRECTION('ref_axis',(-0.479425538604204,0.,0.877582561890372)) ;
#5538 = DIRECTION('center_axis',(0.,-1.,0.)) ;
#5539 = DIRECTION('ref_axis',(0.,0.,1.)) ;
#5540 = DIRECTION('center_axis',(0.,-1.,0.)) ;
#5541 = DIRECTION('ref_axis',(0.479425538604204,0.,-0.877582561890372)) ;
#5542 = DIRECTION('',(0.,1.,0.)) ;
#5543 = DIRECTION('center_axis',(0.,-1.,0.)) ;
#5544 = DIRECTION('ref_axis',(0.,0.,1.)) ;
#5545 = DIRECTION('center_axis',(0.,-1.,0.)) ;
#5546 = DIRECTION('ref_axis',(0.479425538604204,0.,-0.877582561890372)) ;
#5547 = DIRECTION('',(0.339005049420894,0.707106781186865,-0.620544580563467)) ;
#5548 = DIRECTION('axis',(0.,0.,1.)) ;
#5549 = DIRECTION('refdir',(1.,0.,0.)) ;
#5550 = DIRECTION('center_axis',(1.,0.,-1.53837014911E-16)) ;
#5551 = DIRECTION('ref_axis',(-1.53837014911E-16,0.,-1.)) ;
#5552 = DIRECTION('',(0.,1.,0.)) ;
#5553 = DIRECTION('',(0.,0.,-1.)) ;
#5554 = DIRECTION('',(0.,1.,0.)) ;
#5555 = DIRECTION('',(0.,0.,-1.)) ;
#5556 = DIRECTION('center_axis',(0.50000000000019,0.,-0.866025403784329)) ;
#5557 = DIRECTION('ref_axis',(-0.866025403784329,0.,-0.50000000000019)) ;
#5558 = DIRECTION('',(0.,1.,0.)) ;
#5559 = DIRECTION('',(-0.866025403784329,0.,-0.50000000000019)) ;
#5560 = DIRECTION('',(-0.866025403784329,0.,-0.50000000000019)) ;
#5561 = DIRECTION('center_axis',(0.50000000000019,0.,0.866025403784329)) ;
#5562 = DIRECTION('ref_axis',(0.866025403784329,0.,-0.50000000000019)) ;
#5563 = DIRECTION('',(0.866025403784329,0.,-0.50000000000019)) ;
#5564 = DIRECTION('',(0.,1.,0.)) ;
#5565 = DIRECTION('',(0.866025403784329,0.,-0.50000000000019)) ;
#5566 = DIRECTION('center_axis',(0.,-1.,0.)) ;
#5567 = DIRECTION('ref_axis',(1.,0.,0.)) ;
#5568 = DIRECTION('',(0.866025403784329,0.,0.50000000000019)) ;
#5569 = DIRECTION('',(0.,0.,1.)) ;
#5570 = DIRECTION('',(-0.866025403784329,0.,0.50000000000019)) ;
#5571 = DIRECTION('center_axis',(-0.50000000000019,0.,-0.866025403784329)) ;
#5572 = DIRECTION('ref_axis',(-0.866025403784329,0.,0.50000000000019)) ;
#5573 = DIRECTION('',(0.,1.,0.)) ;
#5574 = DIRECTION('',(-0.866025403784329,0.,0.50000000000019)) ;
#5575 = DIRECTION('center_axis',(-0.50000000000019,0.,0.866025403784329)) ;
#5576 = DIRECTION('ref_axis',(0.866025403784329,0.,0.50000000000019)) ;
#5577 = DIRECTION('',(0.866025403784329,0.,0.50000000000019)) ;
#5578 = DIRECTION('',(0.,1.,0.)) ;
#5579 = DIRECTION('center_axis',(-1.,0.,0.)) ;
#5580 = DIRECTION('ref_axis',(0.,0.,1.)) ;
#5581 = DIRECTION('',(0.,0.,1.)) ;
#5582 = DIRECTION('center_axis',(0.,-1.,0.)) ;
#5583 = DIRECTION('ref_axis',(-1.,0.,0.)) ;
#5584 = DIRECTION('center_axis',(0.,-1.,0.)) ;
#5585 = DIRECTION('ref_axis',(0.,0.,1.)) ;
#5586 = DIRECTION('center_axis',(0.,-1.,0.)) ;
#5587 = DIRECTION('ref_axis',(-1.,0.,0.)) ;
#5588 = DIRECTION('center_axis',(0.,-1.,0.)) ;
#5589 = DIRECTION('ref_axis',(0.,0.,1.)) ;
#5590 = DIRECTION('center_axis',(0.,-1.,0.)) ;
#5591 = DIRECTION('ref_axis',(0.,0.,1.)) ;
#5592 = DIRECTION('center_axis',(0.,-1.,0.)) ;
#5593 = DIRECTION('ref_axis',(-1.,0.,0.)) ;
#5594 = DIRECTION('center_axis',(0.,-1.,0.)) ;
#5595 = DIRECTION('ref_axis',(0.,0.,1.)) ;
#5596 = DIRECTION('center_axis',(0.,-1.,0.)) ;
#5597 = DIRECTION('ref_axis',(0.479425538604205,0.,-0.877582561890372)) ;
#5598 = DIRECTION('center_axis',(-0.877582561890372,0.,-0.479425538604205)) ;
#5599 = DIRECTION('ref_axis',(-0.479425538604205,0.,0.877582561890372)) ;
#5600 = DIRECTION('center_axis',(0.,-1.,0.)) ;
#5601 = DIRECTION('ref_axis',(0.,0.,1.)) ;
#5602 = DIRECTION('center_axis',(0.,-1.,0.)) ;
#5603 = DIRECTION('ref_axis',(0.479425538604204,0.,-0.877582561890372)) ;
#5604 = DIRECTION('',(0.,1.,0.)) ;
#5605 = DIRECTION('center_axis',(0.,-1.,0.)) ;
#5606 = DIRECTION('ref_axis',(0.479425538604204,0.,-0.877582561890372)) ;
#5607 = DIRECTION('center_axis',(0.877582561890372,0.,0.479425538604204)) ;
#5608 = DIRECTION('ref_axis',(-0.479425538604204,0.,0.877582561890372)) ;
#5609 = DIRECTION('center_axis',(0.,-1.,0.)) ;
#5610 = DIRECTION('ref_axis',(0.,0.,1.)) ;
#5611 = DIRECTION('center_axis',(0.,-1.,0.)) ;
#5612 = DIRECTION('ref_axis',(0.479425538604204,0.,-0.877582561890372)) ;
#5613 = DIRECTION('',(0.,1.,0.)) ;
#5614 = DIRECTION('center_axis',(0.,-1.,0.)) ;
#5615 = DIRECTION('ref_axis',(0.,0.,1.)) ;
#5616 = DIRECTION('center_axis',(0.,-1.,0.)) ;
#5617 = DIRECTION('ref_axis',(0.479425538604204,0.,-0.877582561890372)) ;
#5618 = DIRECTION('',(0.339005049420894,0.707106781186865,-0.620544580563467)) ;
#5619 = DIRECTION('',(0.,0.,1.)) ;
#5620 = DIRECTION('',(1.,0.,0.)) ;
#5621 = DIRECTION('',(0.,0.,1.)) ;
#5622 = DIRECTION('',(1.,0.,0.)) ;
#5623 = DIRECTION('',(0.,0.,1.)) ;
#5624 = DIRECTION('',(1.,0.,0.)) ;
#5625 = DIRECTION('',(0.,0.,1.)) ;
#5626 = DIRECTION('',(1.,0.,0.)) ;
#5627 = DIRECTION('',(0.,0.,1.)) ;
#5628 = DIRECTION('',(1.,0.,0.)) ;
#5629 = DIRECTION('',(0.,0.,1.)) ;
#5630 = DIRECTION('',(1.,0.,0.)) ;
#5631 = DIRECTION('',(0.,0.,1.)) ;
#5632 = DIRECTION('',(1.,0.,0.)) ;
#5633 = DIRECTION('',(0.,0.,1.)) ;
#5634 = DIRECTION('',(1.,0.,0.)) ;
#5635 = DIRECTION('',(0.,0.,1.)) ;
#5636 = DIRECTION('',(1.,0.,0.)) ;
#5637 = DIRECTION('',(0.,0.,1.)) ;
#5638 = DIRECTION('',(1.,0.,0.)) ;
#5639 = CARTESIAN_POINT('',(0.,0.,0.)) ;
#5640 = CARTESIAN_POINT('',(0.,0.,0.)) ;
#5641 = CARTESIAN_POINT('Origin',(0.,0.,0.)) ;
#5642 = CARTESIAN_POINT('',(-27.477991193,1.1,-19.)) ;
#5643 = CARTESIAN_POINT('',(27.477991193,1.1,-19.)) ;
#5644 = CARTESIAN_POINT('Origin',(0.,0.,-19.)) ;
#5645 = CARTESIAN_POINT('',(27.477991193,1.1,19.)) ;
#5646 = CARTESIAN_POINT('',(27.477991193,1.1,0.)) ;
#5647 = CARTESIAN_POINT('',(-27.477991193,1.1,19.)) ;
#5648 = CARTESIAN_POINT('Origin',(0.,0.,19.)) ;
#5649 = CARTESIAN_POINT('',(-27.477991193,1.1,0.)) ;
#5650 = CARTESIAN_POINT('Origin',(1.46549439250795E-13,-7.50510764646976E-14,
7.4999999999991)) ;
#5651 = CARTESIAN_POINT('',(28.4787640181,1.1,-20.)) ;
#5652 = CARTESIAN_POINT('Ctrl Pts',(27.477991192964,1.1,-19.0000000000358)) ;
#5653 = CARTESIAN_POINT('Ctrl Pts',(27.969442133948,1.1,-19.4910576228772)) ;
#5654 = CARTESIAN_POINT('Ctrl Pts',(28.4787640182424,1.1,-20.0000000001439)) ;
#5655 = CARTESIAN_POINT('',(-28.4787640181,1.1,-20.)) ;
#5656 = CARTESIAN_POINT('Ctrl Pts',(-27.4779911929642,1.1,-19.0000000000358)) ;
#5657 = CARTESIAN_POINT('Ctrl Pts',(-27.9694421338791,1.1,-19.4910576228081)) ;
#5658 = CARTESIAN_POINT('Ctrl Pts',(-28.4787640180994,1.1,-20.0000000000006)) ;
#5659 = CARTESIAN_POINT('Origin',(8.5828066488E-28,-1.7763568394E-15,-20.)) ;
#5660 = CARTESIAN_POINT('Origin',(1.46549439250795E-13,-7.50510764646976E-14,
-7.4999999999991)) ;
#5661 = CARTESIAN_POINT('',(-28.4787640181,1.1,20.)) ;
#5662 = CARTESIAN_POINT('',(28.4787640181,1.1,20.)) ;
#5663 = CARTESIAN_POINT('Origin',(8.5828066488E-28,-1.7763568394E-15,20.)) ;
#5664 = CARTESIAN_POINT('Ctrl Pts',(-27.4779911929643,1.10000000000001,19.0000000000358)) ;
#5665 = CARTESIAN_POINT('Ctrl Pts',(-27.9694421339483,1.1,19.4910576228773)) ;
#5666 = CARTESIAN_POINT('Ctrl Pts',(-28.4787640182428,1.1,20.0000000001439)) ;
#5667 = CARTESIAN_POINT('Ctrl Pts',(27.4779911929641,1.1,19.0000000000359)) ;
#5668 = CARTESIAN_POINT('Ctrl Pts',(27.969442133879,1.1,19.4910576228083)) ;
#5669 = CARTESIAN_POINT('Ctrl Pts',(28.4787640180992,1.1,20.0000000000008)) ;
#5670 = CARTESIAN_POINT('Origin',(35.,1.2,10.)) ;
#5671 = CARTESIAN_POINT('',(32.1478566739,1.1,11.5581330005)) ;
#5672 = CARTESIAN_POINT('Origin',(35.,1.1,10.)) ;
#5673 = CARTESIAN_POINT('',(32.1478566739,33.1,11.5581330005)) ;
#5674 = CARTESIAN_POINT('',(32.1478566738563,1.2,11.5581330004637)) ;
#5675 = CARTESIAN_POINT('Origin',(35.,33.1,10.)) ;
#5676 = CARTESIAN_POINT('Origin',(34.9999999999999,30.8499999999989,10.0000000000002)) ;
#5677 = CARTESIAN_POINT('',(31.6213071102,33.7,11.845788275)) ;
#5678 = CARTESIAN_POINT('',(34.1224174381095,30.8499999999987,10.4794255386044)) ;
#5679 = CARTESIAN_POINT('Origin',(35.,33.7,10.)) ;
#5680 = CARTESIAN_POINT('Origin',(35.,1.2,-10.)) ;
#5681 = CARTESIAN_POINT('',(32.1478566739,1.1,-8.44186699954)) ;
#5682 = CARTESIAN_POINT('Origin',(35.,1.1,-10.)) ;
#5683 = CARTESIAN_POINT('',(32.1478566739,33.1,-8.44186699954)) ;
#5684 = CARTESIAN_POINT('',(32.1478566738563,1.2,-8.44186699953634)) ;
#5685 = CARTESIAN_POINT('Origin',(35.,33.1,-10.)) ;
#5686 = CARTESIAN_POINT('Origin',(34.9999999999999,30.8499999999989,-9.99999999999983)) ;
#5687 = CARTESIAN_POINT('',(31.6213071102,33.7,-8.15421172498)) ;
#5688 = CARTESIAN_POINT('',(34.1224174381095,30.8499999999987,-9.52057446139563)) ;
#5689 = CARTESIAN_POINT('Origin',(35.,33.7,-10.)) ;
#5690 = CARTESIAN_POINT('Origin',(-35.,1.2,10.)) ;
#5691 = CARTESIAN_POINT('',(-37.8521433261,1.1,11.5581330005)) ;
#5692 = CARTESIAN_POINT('Origin',(-35.,1.1,10.)) ;
#5693 = CARTESIAN_POINT('',(-37.8521433261,33.1,11.5581330005)) ;
#5694 = CARTESIAN_POINT('',(-37.8521433261437,1.2,11.5581330004637)) ;
#5695 = CARTESIAN_POINT('Origin',(-35.,33.1,10.)) ;
#5696 = CARTESIAN_POINT('Origin',(-35.0000000000001,30.8499999999989,10.0000000000002)) ;
#5697 = CARTESIAN_POINT('',(-38.3786928898,33.7,11.845788275)) ;
#5698 = CARTESIAN_POINT('',(-35.8775825618905,30.8499999999987,10.4794255386044)) ;
#5699 = CARTESIAN_POINT('Origin',(-35.,33.7,10.)) ;
#5700 = CARTESIAN_POINT('Origin',(-35.,1.2,-10.)) ;
#5701 = CARTESIAN_POINT('',(-37.8521433261,1.1,-8.44186699954)) ;
#5702 = CARTESIAN_POINT('Origin',(-35.,1.1,-10.)) ;
#5703 = CARTESIAN_POINT('',(-37.8521433261,33.1,-8.44186699954)) ;
#5704 = CARTESIAN_POINT('',(-37.8521433261437,1.2,-8.44186699953634)) ;
#5705 = CARTESIAN_POINT('Origin',(-35.,33.1,-10.)) ;
#5706 = CARTESIAN_POINT('Origin',(-35.0000000000001,30.8499999999989,-9.99999999999982)) ;
#5707 = CARTESIAN_POINT('',(-38.3786928898,33.7,-8.15421172498)) ;
#5708 = CARTESIAN_POINT('',(-35.8775825618905,30.8499999999987,-9.52057446139562)) ;
#5709 = CARTESIAN_POINT('Origin',(-35.,33.7,-10.)) ;
#5710 = CARTESIAN_POINT('Origin',(0.,0.,20.)) ;
#5711 = CARTESIAN_POINT('',(-41.85,1.1,20.)) ;
#5712 = CARTESIAN_POINT('',(-35.1643820091,1.1,20.)) ;
#5713 = CARTESIAN_POINT('',(41.85,1.1,20.)) ;
#5714 = CARTESIAN_POINT('',(35.1643820091,1.1,20.)) ;
#5715 = CARTESIAN_POINT('',(41.8500001209205,13.3686291499579,19.9999998790792)) ;
#5716 = CARTESIAN_POINT('',(41.85,7.23431457505,20.)) ;
#5717 = CARTESIAN_POINT('',(42.2600505063,14.3585786438,20.)) ;
#5718 = CARTESIAN_POINT('Origin',(43.2499986516453,13.3686300510977,19.9999984095153)) ;
#5719 = CARTESIAN_POINT('',(44.4,16.4985281374,20.)) ;
#5720 = CARTESIAN_POINT('',(43.3300252532,15.4285533906,20.)) ;
#5721 = CARTESIAN_POINT('',(44.4,31.4514718626,20.)) ;
#5722 = CARTESIAN_POINT('',(44.4,23.975,20.)) ;
#5723 = CARTESIAN_POINT('',(42.7514718626,33.1,20.)) ;
#5724 = CARTESIAN_POINT('',(43.5757359313,32.2757359313,20.)) ;
#5725 = CARTESIAN_POINT('',(25.2485281374,33.1,20.)) ;
#5726 = CARTESIAN_POINT('',(34.,33.1,20.)) ;
#5727 = CARTESIAN_POINT('',(23.6585785583632,31.5100505919387,19.9999998790932)) ;
#5728 = CARTESIAN_POINT('',(24.4535533906,32.3050252532,20.)) ;
#5729 = CARTESIAN_POINT('',(22.6686291501,31.1,20.)) ;
#5730 = CARTESIAN_POINT('Origin',(22.6686294664262,32.4999984096667,19.9999984096869)) ;
#5731 = CARTESIAN_POINT('',(11.0713708500427,31.1000001209203,19.9999998790789)) ;
#5732 = CARTESIAN_POINT('',(16.87,31.1,20.)) ;
#5733 = CARTESIAN_POINT('',(10.0814213562,31.5100505063,20.)) ;
#5734 = CARTESIAN_POINT('Origin',(11.0713699489153,32.4999986516766,19.9999984095466)) ;
#5735 = CARTESIAN_POINT('',(8.49147186258,33.1,20.)) ;
#5736 = CARTESIAN_POINT('',(9.28644660941,32.3050252532,20.)) ;
#5737 = CARTESIAN_POINT('',(-8.49147186258,33.1,20.)) ;
#5738 = CARTESIAN_POINT('',(3.5527136788E-14,33.1,20.)) ;
#5739 = CARTESIAN_POINT('',(-10.0814213562,31.5100505063,20.)) ;
#5740 = CARTESIAN_POINT('',(-9.28644660941,32.3050252532,20.)) ;
#5741 = CARTESIAN_POINT('',(-11.0713708496686,31.100000074351,19.9999999256495)) ;
#5742 = CARTESIAN_POINT('Origin',(-11.0713702946003,32.4999991690532,19.999999019805)) ;
#5743 = CARTESIAN_POINT('',(-22.6686291501,31.1,20.)) ;
#5744 = CARTESIAN_POINT('',(-16.87,31.1,20.)) ;
#5745 = CARTESIAN_POINT('',(-23.6585785910206,31.5100505587523,19.9999999256531)) ;
#5746 = CARTESIAN_POINT('Origin',(-22.6686293450353,32.4999990198376,19.9999990198396)) ;
#5747 = CARTESIAN_POINT('',(-25.2485281374,33.1,20.)) ;
#5748 = CARTESIAN_POINT('',(-24.4535533906,32.3050252532,20.)) ;
#5749 = CARTESIAN_POINT('',(-42.7514718626,33.1,20.)) ;
#5750 = CARTESIAN_POINT('',(-34.,33.1,20.)) ;
#5751 = CARTESIAN_POINT('',(-44.4,31.4514718626,20.)) ;
#5752 = CARTESIAN_POINT('',(-43.5757359313,32.2757359313,20.)) ;
#5753 = CARTESIAN_POINT('',(-44.4,16.4985281374,20.)) ;
#5754 = CARTESIAN_POINT('',(-44.4,23.975,20.)) ;
#5755 = CARTESIAN_POINT('',(-42.2600505063,14.3585786438,20.)) ;
#5756 = CARTESIAN_POINT('',(-43.3300252532,15.4285533906,20.)) ;
#5757 = CARTESIAN_POINT('',(-41.8500000743509,13.3686291503314,19.9999999256495)) ;
#5758 = CARTESIAN_POINT('Origin',(-43.2499991690533,13.3686297053997,19.9999990198052)) ;
#5759 = CARTESIAN_POINT('',(-41.85,7.23431457505,20.)) ;
#5760 = CARTESIAN_POINT('Origin',(43.2499999999937,13.3686291501029,19.6000000000109)) ;
#5761 = CARTESIAN_POINT('',(42.45,13.3686291501,19.4)) ;
#5762 = CARTESIAN_POINT('',(42.15,13.3686291501,19.7)) ;
#5763 = CARTESIAN_POINT('',(42.6843145751,13.9343145751,19.4)) ;
#5764 = CARTESIAN_POINT('Origin',(43.25,13.3686291501,19.4)) ;
#5765 = CARTESIAN_POINT('',(42.4721825407,14.1464466094,19.7)) ;
#5766 = CARTESIAN_POINT('Origin',(22.9057359313,-5.84426406871,19.4)) ;
#5767 = CARTESIAN_POINT('',(44.8242640687,16.0742640687,19.4)) ;
#5768 = CARTESIAN_POINT('',(43.165,14.415,19.4)) ;
#5769 = CARTESIAN_POINT('',(44.6121320344,16.2863961031,19.7)) ;
#5770 = CARTESIAN_POINT('Origin',(44.4,16.4985281374,18.9999999999991)) ;
#5771 = CARTESIAN_POINT('',(45.,16.4985281374,19.4)) ;
#5772 = CARTESIAN_POINT('Origin',(44.4,16.4985281374,19.4)) ;
#5773 = CARTESIAN_POINT('',(44.7,16.4985281374,19.7)) ;
#5774 = CARTESIAN_POINT('Origin',(45.,-5.42,19.4)) ;
#5775 = CARTESIAN_POINT('',(45.,31.4514718626,19.4)) ;
#5776 = CARTESIAN_POINT('',(45.,17.4,19.4)) ;
#5777 = CARTESIAN_POINT('',(44.7,31.4514718626,19.7)) ;
#5778 = CARTESIAN_POINT('Origin',(44.4,31.4514718626,18.9999999999991)) ;
#5779 = CARTESIAN_POINT('',(44.8242640687,31.8757359313,19.4)) ;
#5780 = CARTESIAN_POINT('Origin',(44.4,31.4514718626,19.4)) ;
#5781 = CARTESIAN_POINT('',(44.6121320344,31.6636038969,19.7)) ;
#5782 = CARTESIAN_POINT('Origin',(36.0557359313,40.6442640687,19.4)) ;
#5783 = CARTESIAN_POINT('',(43.1757359313,33.5242640687,19.4)) ;
#5784 = CARTESIAN_POINT('',(49.74,26.96,19.4)) ;
#5785 = CARTESIAN_POINT('',(42.9636038969,33.3121320344,19.7)) ;
#5786 = CARTESIAN_POINT('Origin',(42.7514718626,33.1,18.9999999999991)) ;
#5787 = CARTESIAN_POINT('',(42.7514718626,33.7,19.4)) ;
#5788 = CARTESIAN_POINT('Origin',(42.7514718626,33.1,19.4)) ;
#5789 = CARTESIAN_POINT('',(42.7514718626,33.4,19.7)) ;
#5790 = CARTESIAN_POINT('Origin',(-63.,33.7,19.4)) ;
#5791 = CARTESIAN_POINT('',(25.2485281374,33.7,19.4)) ;
#5792 = CARTESIAN_POINT('',(0.,33.7,19.4)) ;
#5793 = CARTESIAN_POINT('',(25.2485281374,33.4,19.7)) ;
#5794 = CARTESIAN_POINT('Origin',(25.2485281374,33.1,18.9999999999991)) ;
#5795 = CARTESIAN_POINT('',(24.8242640687,33.5242640687,19.4)) ;
#5796 = CARTESIAN_POINT('Origin',(25.2485281374,33.1,19.4)) ;
#5797 = CARTESIAN_POINT('',(25.0363961031,33.3121320344,19.7)) ;
#5798 = CARTESIAN_POINT('Origin',(-13.6957359313,-4.99573593129,19.4)) ;
#5799 = CARTESIAN_POINT('',(23.2343145751,31.9343145751,19.4)) ;
#5800 = CARTESIAN_POINT('',(9.12426406871,17.8242640687,19.4)) ;
#5801 = CARTESIAN_POINT('',(23.4464466094,31.7221825407,19.7)) ;
#5802 = CARTESIAN_POINT('Origin',(22.6686291501024,32.4999999999935,19.6000000000109)) ;
#5803 = CARTESIAN_POINT('',(22.6686291501,31.7,19.4)) ;
#5804 = CARTESIAN_POINT('Origin',(22.6686291501,32.5,19.4)) ;
#5805 = CARTESIAN_POINT('',(22.6686291501,31.4,19.7)) ;
#5806 = CARTESIAN_POINT('Origin',(-63.,31.7,19.4)) ;
#5807 = CARTESIAN_POINT('',(11.0713708499,31.7,19.4)) ;
#5808 = CARTESIAN_POINT('',(0.,31.7,19.4)) ;
#5809 = CARTESIAN_POINT('',(11.0713708499,31.4,19.7)) ;
#5810 = CARTESIAN_POINT('Origin',(11.0713708498971,32.4999999999937,19.6000000000109)) ;
#5811 = CARTESIAN_POINT('',(10.5056854249,31.9343145751,19.4)) ;
#5812 = CARTESIAN_POINT('Origin',(11.0713708499,32.5,19.4)) ;
#5813 = CARTESIAN_POINT('',(10.2935533906,31.7221825407,19.7)) ;
#5814 = CARTESIAN_POINT('Origin',(1.79573593129,40.6442640687,19.4)) ;
#5815 = CARTESIAN_POINT('',(8.91573593129,33.5242640687,19.4)) ;
#5816 = CARTESIAN_POINT('',(24.6157359313,17.8242640687,19.4)) ;
#5817 = CARTESIAN_POINT('',(8.70360389693,33.3121320344,19.7)) ;
#5818 = CARTESIAN_POINT('Origin',(8.49147186258,33.1,18.9999999999991)) ;
#5819 = CARTESIAN_POINT('',(8.49147186258,33.7,19.4)) ;
#5820 = CARTESIAN_POINT('Origin',(8.49147186258,33.1,19.4)) ;
#5821 = CARTESIAN_POINT('',(8.49147186258,33.4,19.7)) ;
#5822 = CARTESIAN_POINT('Origin',(-63.,33.7,19.4)) ;
#5823 = CARTESIAN_POINT('',(-8.49147186258,33.7,19.4)) ;
#5824 = CARTESIAN_POINT('',(0.,33.7,19.4)) ;
#5825 = CARTESIAN_POINT('',(-8.49147186258,33.4,19.7)) ;
#5826 = CARTESIAN_POINT('Origin',(-8.49147186258,33.1,18.9999999999991)) ;
#5827 = CARTESIAN_POINT('',(-8.91573593129,33.5242640687,19.4)) ;
#5828 = CARTESIAN_POINT('Origin',(-8.49147186258,33.1,19.4)) ;
#5829 = CARTESIAN_POINT('',(-8.70360389693,33.3121320344,19.7)) ;
#5830 = CARTESIAN_POINT('Origin',(-1.79573593129,40.6442640687,19.4)) ;
#5831 = CARTESIAN_POINT('',(-10.5056854249,31.9343145751,19.4)) ;
#5832 = CARTESIAN_POINT('',(-24.6157359313,17.8242640687,19.4)) ;
#5833 = CARTESIAN_POINT('',(-10.2935533906,31.7221825407,19.7)) ;
#5834 = CARTESIAN_POINT('Origin',(-11.0713708499,32.5,19.6000000000009)) ;
#5835 = CARTESIAN_POINT('',(-11.0713708499,31.7,19.4)) ;
#5836 = CARTESIAN_POINT('Origin',(-11.0713708499,32.5,19.4)) ;
#5837 = CARTESIAN_POINT('',(-11.0713708499,31.4,19.7)) ;
#5838 = CARTESIAN_POINT('Origin',(-63.,31.7,19.4)) ;
#5839 = CARTESIAN_POINT('',(-22.6686291501,31.7,19.4)) ;
#5840 = CARTESIAN_POINT('',(0.,31.7,19.4)) ;
#5841 = CARTESIAN_POINT('',(-22.6686291501,31.4,19.7)) ;
#5842 = CARTESIAN_POINT('Origin',(-22.6686291501,32.5,19.6000000000009)) ;
#5843 = CARTESIAN_POINT('',(-23.2343145751,31.9343145751,19.4)) ;
#5844 = CARTESIAN_POINT('Origin',(-22.6686291501,32.5,19.4)) ;
#5845 = CARTESIAN_POINT('',(-23.4464466094,31.7221825407,19.7)) ;
#5846 = CARTESIAN_POINT('Origin',(13.6957359313,-4.99573593129,19.4)) ;
#5847 = CARTESIAN_POINT('',(-24.8242640687,33.5242640687,19.4)) ;
#5848 = CARTESIAN_POINT('',(-9.12426406871,17.8242640687,19.4)) ;
#5849 = CARTESIAN_POINT('',(-25.0363961031,33.3121320344,19.7)) ;
#5850 = CARTESIAN_POINT('Origin',(-25.2485281374,33.1000000000001,18.9999999999991)) ;
#5851 = CARTESIAN_POINT('',(-25.2485281374,33.7,19.4)) ;
#5852 = CARTESIAN_POINT('Origin',(-25.2485281374,33.1,19.4)) ;
#5853 = CARTESIAN_POINT('',(-25.2485281374,33.4,19.7)) ;
#5854 = CARTESIAN_POINT('Origin',(-63.,33.7,19.4)) ;
#5855 = CARTESIAN_POINT('',(-42.7514718626,33.7,19.4)) ;
#5856 = CARTESIAN_POINT('',(0.,33.7,19.4)) ;
#5857 = CARTESIAN_POINT('',(-42.7514718626,33.4,19.7)) ;
#5858 = CARTESIAN_POINT('Origin',(-42.7514718626,33.1,18.9999999999991)) ;
#5859 = CARTESIAN_POINT('',(-43.1757359313,33.5242640687,19.4)) ;
#5860 = CARTESIAN_POINT('Origin',(-42.7514718626,33.1,19.4)) ;
#5861 = CARTESIAN_POINT('',(-42.9636038969,33.3121320344,19.7)) ;
#5862 = CARTESIAN_POINT('Origin',(-43.1757359313,33.5242640687,19.4)) ;
#5863 = CARTESIAN_POINT('',(-44.8242640687,31.8757359313,19.4)) ;
#5864 = CARTESIAN_POINT('',(-53.3,23.4,19.4)) ;
#5865 = CARTESIAN_POINT('',(-44.6121320344,31.6636038969,19.7)) ;
#5866 = CARTESIAN_POINT('Origin',(-44.4,31.4514718626,18.9999999999991)) ;
#5867 = CARTESIAN_POINT('',(-45.,31.4514718626,19.4)) ;
#5868 = CARTESIAN_POINT('Origin',(-44.4,31.4514718626,19.4)) ;
#5869 = CARTESIAN_POINT('',(-44.7,31.4514718626,19.7)) ;
#5870 = CARTESIAN_POINT('Origin',(-45.,-5.42,19.4)) ;
#5871 = CARTESIAN_POINT('',(-45.,16.4985281374,19.4)) ;
#5872 = CARTESIAN_POINT('',(-45.,17.4,19.4)) ;
#5873 = CARTESIAN_POINT('',(-44.7,16.4985281374,19.7)) ;
#5874 = CARTESIAN_POINT('Origin',(-44.4,16.4985281374,18.9999999999991)) ;
#5875 = CARTESIAN_POINT('',(-44.8242640687,16.0742640687,19.4)) ;
#5876 = CARTESIAN_POINT('Origin',(-44.4,16.4985281374,19.4)) ;
#5877 = CARTESIAN_POINT('',(-44.6121320344,16.2863961031,19.7)) ;
#5878 = CARTESIAN_POINT('Origin',(-22.9057359313,-5.84426406871,19.4)) ;
#5879 = CARTESIAN_POINT('',(-42.6843145751,13.9343145751,19.4)) ;
#5880 = CARTESIAN_POINT('',(-33.865,5.115,19.4)) ;
#5881 = CARTESIAN_POINT('',(-42.4721825407,14.1464466094,19.7)) ;
#5882 = CARTESIAN_POINT('Origin',(-43.25,13.3686291501,19.6000000000009)) ;
#5883 = CARTESIAN_POINT('',(-42.45,13.3686291501,19.4)) ;
#5884 = CARTESIAN_POINT('Origin',(-43.25,13.3686291501,19.4)) ;
#5885 = CARTESIAN_POINT('',(-42.15,13.3686291501,19.7)) ;
#5886 = CARTESIAN_POINT('Origin',(-42.45,-5.42,19.4)) ;
#5887 = CARTESIAN_POINT('',(-42.45,1.1,19.4)) ;
#5888 = CARTESIAN_POINT('',(-42.15,1.1,19.7)) ;
#5889 = CARTESIAN_POINT('',(-42.45,3.97431457505,19.4)) ;
#5890 = CARTESIAN_POINT('Origin',(42.45,-5.42,19.4)) ;
#5891 = CARTESIAN_POINT('',(42.45,1.1,19.4)) ;
#5892 = CARTESIAN_POINT('',(42.45,17.4,19.4)) ;
#5893 = CARTESIAN_POINT('',(42.15,1.1,19.7)) ;
#5894 = CARTESIAN_POINT('Origin',(0.,0.,-20.)) ;
#5895 = CARTESIAN_POINT('',(-41.8500000743509,13.3686292513994,-19.9999999256495)) ;
#5896 = CARTESIAN_POINT('',(-41.85,1.1,-20.)) ;
#5897 = CARTESIAN_POINT('',(-41.85,7.23431457505,-20.)) ;
#5898 = CARTESIAN_POINT('',(-42.2600505063,14.3585786438,-20.)) ;
#5899 = CARTESIAN_POINT('Origin',(-43.2499991690534,13.3686297053996,-19.9999990198051)) ;
#5900 = CARTESIAN_POINT('',(-44.4,16.4985281374,-20.)) ;
#5901 = CARTESIAN_POINT('',(-43.3300252532,15.4285533906,-20.)) ;
#5902 = CARTESIAN_POINT('',(-44.4,31.4514718626,-20.)) ;
#5903 = CARTESIAN_POINT('',(-44.4,23.975,-20.)) ;
#5904 = CARTESIAN_POINT('',(-42.7514718626,33.1,-20.)) ;
#5905 = CARTESIAN_POINT('',(-43.5757359313,32.2757359313,-20.)) ;
#5906 = CARTESIAN_POINT('',(-25.2485281374,33.1,-20.)) ;
#5907 = CARTESIAN_POINT('',(-34.,33.1,-20.)) ;
#5908 = CARTESIAN_POINT('',(-23.6585785195402,31.510050487272,-19.9999999256531)) ;
#5909 = CARTESIAN_POINT('',(-24.4535533906,32.3050252532,-20.)) ;
#5910 = CARTESIAN_POINT('',(-22.6686291501,31.1,-20.)) ;
#5911 = CARTESIAN_POINT('Origin',(-22.6686293450353,32.4999990198376,-19.9999990198394)) ;
#5912 = CARTESIAN_POINT('',(-11.0713707486006,31.1000000743509,-19.9999999256495)) ;
#5913 = CARTESIAN_POINT('',(-16.87,31.1,-20.)) ;
#5914 = CARTESIAN_POINT('',(-10.0814213562,31.5100505063,-20.)) ;
#5915 = CARTESIAN_POINT('Origin',(-11.0713702946003,32.4999991690532,-19.999999019805)) ;
#5916 = CARTESIAN_POINT('',(-8.49147186258,33.1,-20.)) ;
#5917 = CARTESIAN_POINT('',(-9.28644660941,32.3050252532,-20.)) ;
#5918 = CARTESIAN_POINT('',(8.49147186258,33.1,-20.)) ;
#5919 = CARTESIAN_POINT('',(2.48689957516E-14,33.1,-20.)) ;
#5920 = CARTESIAN_POINT('',(10.0814213562,31.5100505063,-20.)) ;
#5921 = CARTESIAN_POINT('',(9.28644660941,32.3050252532,-20.)) ;
#5922 = CARTESIAN_POINT('',(11.0713708500427,31.1000001209198,-19.9999998790785)) ;
#5923 = CARTESIAN_POINT('Origin',(11.071369948907,32.4999986516472,-19.9999984095746)) ;
#5924 = CARTESIAN_POINT('',(22.6686291501,31.1,-20.)) ;
#5925 = CARTESIAN_POINT('',(16.87,31.1,-20.)) ;
#5926 = CARTESIAN_POINT('',(23.6585785583635,31.5100505919384,-19.9999998790928)) ;
#5927 = CARTESIAN_POINT('Origin',(22.6686294664411,32.4999984096401,-19.9999984097149)) ;
#5928 = CARTESIAN_POINT('',(25.2485281374,33.1,-20.)) ;
#5929 = CARTESIAN_POINT('',(24.4535533906,32.3050252532,-20.)) ;
#5930 = CARTESIAN_POINT('',(42.7514718626,33.1,-20.)) ;
#5931 = CARTESIAN_POINT('',(34.,33.1,-20.)) ;
#5932 = CARTESIAN_POINT('',(44.4,31.4514718626,-20.)) ;
#5933 = CARTESIAN_POINT('',(43.5757359313,32.2757359313,-20.)) ;
#5934 = CARTESIAN_POINT('',(44.4,16.4985281374,-20.)) ;
#5935 = CARTESIAN_POINT('',(44.4,23.975,-20.)) ;
#5936 = CARTESIAN_POINT('',(42.2600505063,14.3585786438,-20.)) ;
#5937 = CARTESIAN_POINT('',(43.3300252532,15.4285533906,-20.)) ;
#5938 = CARTESIAN_POINT('',(41.8500001209206,13.3686289388372,-19.9999998790791)) ;
#5939 = CARTESIAN_POINT('Origin',(43.2499986516453,13.3686300510977,-19.9999984095153)) ;
#5940 = CARTESIAN_POINT('',(41.85,1.1,-20.)) ;
#5941 = CARTESIAN_POINT('',(41.85,7.23431457505,-20.)) ;
#5942 = CARTESIAN_POINT('',(35.1643820091,1.1,-20.)) ;
#5943 = CARTESIAN_POINT('',(-35.1643820091,1.1,-20.)) ;
#5944 = CARTESIAN_POINT('Origin',(22.6686291501,32.5,0.)) ;
#5945 = CARTESIAN_POINT('',(23.2343145751,31.9343145751,-19.4)) ;
#5946 = CARTESIAN_POINT('',(22.6686291501,31.7,-19.4)) ;
#5947 = CARTESIAN_POINT('Origin',(22.6686291501,32.5,-19.4)) ;
#5948 = CARTESIAN_POINT('',(22.6686291501,31.7,0.)) ;
#5949 = CARTESIAN_POINT('',(23.2343145751,31.9343145751,0.)) ;
#5950 = CARTESIAN_POINT('Origin',(11.0713708499,32.5,0.)) ;
#5951 = CARTESIAN_POINT('',(11.0713708499,31.7,-19.4)) ;
#5952 = CARTESIAN_POINT('',(10.5056854249,31.9343145751,-19.4)) ;
#5953 = CARTESIAN_POINT('Origin',(11.0713708499,32.5,-19.4)) ;
#5954 = CARTESIAN_POINT('',(10.5056854249,31.9343145751,0.)) ;
#5955 = CARTESIAN_POINT('',(11.0713708499,31.7,0.)) ;
#5956 = CARTESIAN_POINT('Origin',(-11.0713708499,32.5,0.)) ;
#5957 = CARTESIAN_POINT('',(-10.5056854249,31.9343145751,-19.4)) ;
#5958 = CARTESIAN_POINT('',(-11.0713708211758,31.7,-19.4)) ;
#5959 = CARTESIAN_POINT('Origin',(-11.0713708499,32.5,-19.4)) ;
#5960 = CARTESIAN_POINT('',(-11.0713708499,31.7,0.)) ;
#5961 = CARTESIAN_POINT('',(-10.5056854249,31.9343145751,0.)) ;
#5962 = CARTESIAN_POINT('Origin',(-22.6686291501,32.5,0.)) ;
#5963 = CARTESIAN_POINT('',(-22.6686291501,31.7,-19.4)) ;
#5964 = CARTESIAN_POINT('',(-23.2343145547562,31.934314554758,-19.4000000000014)) ;
#5965 = CARTESIAN_POINT('Origin',(-22.6686291501,32.5,-19.4)) ;
#5966 = CARTESIAN_POINT('',(-23.2343145751,31.9343145751,0.)) ;
#5967 = CARTESIAN_POINT('',(-22.6686291501,31.7,0.)) ;
#5968 = CARTESIAN_POINT('Origin',(-43.25,13.3686291501,0.)) ;
#5969 = CARTESIAN_POINT('',(-42.6843145751,13.9343145751,-19.4)) ;
#5970 = CARTESIAN_POINT('',(-42.45,13.3686291788242,-19.4)) ;
#5971 = CARTESIAN_POINT('Origin',(-43.25,13.3686291501,-19.4)) ;
#5972 = CARTESIAN_POINT('',(-42.45,13.3686291501,0.)) ;
#5973 = CARTESIAN_POINT('',(-42.6843145751,13.9343145751,0.)) ;
#5974 = CARTESIAN_POINT('Origin',(43.25,13.3686291501,0.)) ;
#5975 = CARTESIAN_POINT('',(42.4499999999998,13.3686290899674,-19.3999999999998)) ;
#5976 = CARTESIAN_POINT('',(42.6843145751,13.9343145751,-19.4)) ;
#5977 = CARTESIAN_POINT('Origin',(43.25,13.3686291501,-19.4)) ;
#5978 = CARTESIAN_POINT('',(42.6843145751,13.9343145751,0.)) ;
#5979 = CARTESIAN_POINT('',(42.45,13.3686291501,0.)) ;
#5980 = CARTESIAN_POINT('Origin',(42.45,13.7,0.)) ;
#5981 = CARTESIAN_POINT('',(42.45,1.1,-19.4)) ;
#5982 = CARTESIAN_POINT('',(42.45,7.23431457505,-19.4)) ;
#5983 = CARTESIAN_POINT('',(42.45,1.1,0.)) ;
#5984 = CARTESIAN_POINT('Origin',(23.,31.7,0.)) ;
#5985 = CARTESIAN_POINT('',(-16.87,31.7,-19.4)) ;
#5986 = CARTESIAN_POINT('Origin',(23.,31.7,0.)) ;
#5987 = CARTESIAN_POINT('',(16.87,31.7,-19.4)) ;
#5988 = CARTESIAN_POINT('Origin',(-42.45,13.7,0.)) ;
#5989 = CARTESIAN_POINT('',(-42.45,1.1,-19.4)) ;
#5990 = CARTESIAN_POINT('',(-42.45,1.1,0.)) ;
#5991 = CARTESIAN_POINT('',(-42.45,7.23431457505,-19.4)) ;
#5992 = CARTESIAN_POINT('Origin',(-42.45,1.1,0.)) ;
#5993 = CARTESIAN_POINT('',(42.15,1.1,-19.7)) ;
#5994 = CARTESIAN_POINT('Origin',(-42.45,1.1,0.)) ;
#5995 = CARTESIAN_POINT('',(-42.15,1.1,-19.7)) ;
#5996 = CARTESIAN_POINT('Origin',(44.4,31.4514718626,0.)) ;
#5997 = CARTESIAN_POINT('',(44.8242640687,31.8757359313,-19.4)) ;
#5998 = CARTESIAN_POINT('',(44.8242640687,31.8757359313,0.)) ;
#5999 = CARTESIAN_POINT('',(45.,31.4514718626,-19.4)) ;
#6000 = CARTESIAN_POINT('',(45.,31.4514718626,0.)) ;
#6001 = CARTESIAN_POINT('Origin',(44.4,31.4514718626,-19.4)) ;
#6002 = CARTESIAN_POINT('Origin',(45.,31.7,0.)) ;
#6003 = CARTESIAN_POINT('',(43.1757359313,33.5242640687,-19.4)) ;
#6004 = CARTESIAN_POINT('',(43.1757359313,33.5242640687,0.)) ;
#6005 = CARTESIAN_POINT('',(44.,32.7,-19.4)) ;
#6006 = CARTESIAN_POINT('Origin',(42.7514718626,33.1,0.)) ;
#6007 = CARTESIAN_POINT('',(42.7514718626,33.7,-19.4)) ;
#6008 = CARTESIAN_POINT('',(42.7514718626,33.7,0.)) ;
#6009 = CARTESIAN_POINT('Origin',(42.7514718626,33.1,-19.4)) ;
#6010 = CARTESIAN_POINT('Origin',(25.,33.7,0.)) ;
#6011 = CARTESIAN_POINT('',(24.8242640687,33.5242640687,-19.4)) ;
#6012 = CARTESIAN_POINT('',(24.8242640687,33.5242640687,0.)) ;
#6013 = CARTESIAN_POINT('',(24.0292893219,32.7292893219,-19.4)) ;
#6014 = CARTESIAN_POINT('Origin',(43.,33.7,0.)) ;
#6015 = CARTESIAN_POINT('',(25.2485281374,33.7,-19.4)) ;
#6016 = CARTESIAN_POINT('',(25.2485281374,33.7,0.)) ;
#6017 = CARTESIAN_POINT('',(34.,33.7,-19.4)) ;
#6018 = CARTESIAN_POINT('Origin',(25.2485281374,33.1,0.)) ;
#6019 = CARTESIAN_POINT('Origin',(25.2485281374,33.1,-19.4)) ;
#6020 = CARTESIAN_POINT('Origin',(10.74,31.7,0.)) ;
#6021 = CARTESIAN_POINT('',(8.91573593129,33.5242640687,-19.4)) ;
#6022 = CARTESIAN_POINT('',(8.91573593129,33.5242640687,0.)) ;
#6023 = CARTESIAN_POINT('',(9.71071067812,32.7292893219,-19.4)) ;
#6024 = CARTESIAN_POINT('Origin',(8.49147186258,33.1,0.)) ;
#6025 = CARTESIAN_POINT('',(8.49147186258,33.7,-19.4)) ;
#6026 = CARTESIAN_POINT('',(8.49147186258,33.7,0.)) ;
#6027 = CARTESIAN_POINT('Origin',(8.49147186258,33.1,-19.4)) ;
#6028 = CARTESIAN_POINT('Origin',(-10.74,31.7,0.)) ;
#6029 = CARTESIAN_POINT('',(-8.91573593129,33.5242640687,-19.4)) ;
#6030 = CARTESIAN_POINT('',(-9.71071067812,32.7292893219,-19.4)) ;
#6031 = CARTESIAN_POINT('',(-8.91573593129,33.5242640687,0.)) ;
#6032 = CARTESIAN_POINT('Origin',(43.,33.7,0.)) ;
#6033 = CARTESIAN_POINT('',(-8.49147186258,33.7,-19.4)) ;
#6034 = CARTESIAN_POINT('',(-8.49147186258,33.7,0.)) ;
#6035 = CARTESIAN_POINT('',(0.,33.7,-19.4)) ;
#6036 = CARTESIAN_POINT('Origin',(-8.49147186258,33.1,0.)) ;
#6037 = CARTESIAN_POINT('Origin',(-8.49147186258,33.1,-19.4)) ;
#6038 = CARTESIAN_POINT('Origin',(-25.,33.7,0.)) ;
#6039 = CARTESIAN_POINT('',(-24.8242640687,33.5242640687,-19.4)) ;
#6040 = CARTESIAN_POINT('',(-24.0292893219,32.7292893219,-19.4)) ;
#6041 = CARTESIAN_POINT('',(-24.8242640687,33.5242640687,0.)) ;
#6042 = CARTESIAN_POINT('Origin',(-25.2485281374,33.1,0.)) ;
#6043 = CARTESIAN_POINT('',(-25.2485281374,33.7,-19.4)) ;
#6044 = CARTESIAN_POINT('',(-25.2485281374,33.7,0.)) ;
#6045 = CARTESIAN_POINT('Origin',(-25.2485281374,33.1,-19.4)) ;
#6046 = CARTESIAN_POINT('Origin',(43.,33.7,0.)) ;
#6047 = CARTESIAN_POINT('',(-42.7514718626,33.7,-19.4)) ;
#6048 = CARTESIAN_POINT('',(-42.7514718626,33.7,0.)) ;
#6049 = CARTESIAN_POINT('',(-34.,33.7,-19.4)) ;
#6050 = CARTESIAN_POINT('Origin',(-42.7514718626,33.1,0.)) ;
#6051 = CARTESIAN_POINT('',(-43.1757359313,33.5242640687,-19.4)) ;
#6052 = CARTESIAN_POINT('',(-43.1757359313,33.5242640687,0.)) ;
#6053 = CARTESIAN_POINT('Origin',(-42.7514718626,33.1,-19.4)) ;
#6054 = CARTESIAN_POINT('Origin',(-45.,31.7,0.)) ;
#6055 = CARTESIAN_POINT('',(-44.8242640687,31.8757359313,-19.4)) ;
#6056 = CARTESIAN_POINT('',(-44.,32.7,-19.4)) ;
#6057 = CARTESIAN_POINT('',(-44.8242640687,31.8757359313,0.)) ;
#6058 = CARTESIAN_POINT('Origin',(-44.4,31.4514718626,0.)) ;
#6059 = CARTESIAN_POINT('',(-45.,31.4514718626,-19.4)) ;
#6060 = CARTESIAN_POINT('',(-45.,31.4514718626,0.)) ;
#6061 = CARTESIAN_POINT('Origin',(-44.4,31.4514718626,-19.4)) ;
#6062 = CARTESIAN_POINT('Origin',(45.,16.25,0.)) ;
#6063 = CARTESIAN_POINT('',(44.8242640687,16.0742640687,-19.4)) ;
#6064 = CARTESIAN_POINT('',(43.7542893219,15.0042893219,-19.4)) ;
#6065 = CARTESIAN_POINT('',(44.8242640687,16.0742640687,0.)) ;
#6066 = CARTESIAN_POINT('Origin',(45.,31.7,0.)) ;
#6067 = CARTESIAN_POINT('',(45.,16.4985281374,-19.4)) ;
#6068 = CARTESIAN_POINT('',(45.,23.975,-19.4)) ;
#6069 = CARTESIAN_POINT('',(45.,16.4985281374,0.)) ;
#6070 = CARTESIAN_POINT('Origin',(44.4,16.4985281374,0.)) ;
#6071 = CARTESIAN_POINT('Origin',(44.4,16.4985281374,-19.4)) ;
#6072 = CARTESIAN_POINT('Origin',(-45.,16.25,0.)) ;
#6073 = CARTESIAN_POINT('',(-44.8242640687,16.0742640687,-19.4)) ;
#6074 = CARTESIAN_POINT('',(-44.8242640687,16.0742640687,0.)) ;
#6075 = CARTESIAN_POINT('',(-43.7542893219,15.0042893219,-19.4)) ;
#6076 = CARTESIAN_POINT('Origin',(-45.,31.7,0.)) ;
#6077 = CARTESIAN_POINT('',(-45.,16.4985281374,-19.4)) ;
#6078 = CARTESIAN_POINT('',(-45.,16.4985281374,0.)) ;
#6079 = CARTESIAN_POINT('',(-45.,23.975,-19.4)) ;
#6080 = CARTESIAN_POINT('Origin',(-44.4,16.4985281374,0.)) ;
#6081 = CARTESIAN_POINT('Origin',(-44.4,16.4985281374,-19.4)) ;
#6082 = CARTESIAN_POINT('Origin',(43.2499999999937,13.3686291501029,-19.6000000000109)) ;
#6083 = CARTESIAN_POINT('',(42.15,13.3686289841,-19.7)) ;
#6084 = CARTESIAN_POINT('',(42.4721825407,14.1464466094,-19.7)) ;
#6085 = CARTESIAN_POINT('Origin',(22.9057359313,-5.84426406871,-19.4)) ;
#6086 = CARTESIAN_POINT('',(44.6121320344,16.2863961031,-19.7)) ;
#6087 = CARTESIAN_POINT('Origin',(44.4,16.4985281374,-18.9999999999991)) ;
#6088 = CARTESIAN_POINT('',(44.7,16.4985281374,-19.7)) ;
#6089 = CARTESIAN_POINT('Origin',(45.,-5.42,-19.4)) ;
#6090 = CARTESIAN_POINT('',(44.7,31.4514718626,-19.7)) ;
#6091 = CARTESIAN_POINT('Origin',(44.4,31.4514718626,-18.9999999999991)) ;
#6092 = CARTESIAN_POINT('',(44.6121320344,31.6636038969,-19.7)) ;
#6093 = CARTESIAN_POINT('Origin',(36.0557359313,40.6442640687,-19.4)) ;
#6094 = CARTESIAN_POINT('',(42.9636038969,33.3121320344,-19.7)) ;
#6095 = CARTESIAN_POINT('Origin',(42.7514718626,33.1,-18.9999999999991)) ;
#6096 = CARTESIAN_POINT('',(42.7514718626,33.4,-19.7)) ;
#6097 = CARTESIAN_POINT('Origin',(-63.,33.7,-19.4)) ;
#6098 = CARTESIAN_POINT('',(25.2485281374,33.4,-19.7)) ;
#6099 = CARTESIAN_POINT('Origin',(25.2485281374,33.1,-18.9999999999991)) ;
#6100 = CARTESIAN_POINT('',(25.0363961031,33.3121320344,-19.7)) ;
#6101 = CARTESIAN_POINT('Origin',(-13.6957359313,-4.99573593129,-19.4)) ;
#6102 = CARTESIAN_POINT('',(23.4464466094,31.7221825407,-19.7)) ;
#6103 = CARTESIAN_POINT('Origin',(22.668629150113,32.4999999999744,-19.6000000000509)) ;
#6104 = CARTESIAN_POINT('',(22.6686291501,31.4,-19.7)) ;
#6105 = CARTESIAN_POINT('Origin',(-63.,31.7,-19.4)) ;
#6106 = CARTESIAN_POINT('',(11.0713708499,31.4,-19.7)) ;
#6107 = CARTESIAN_POINT('Origin',(11.0713708498911,32.4999999999727,-19.6000000000509)) ;
#6108 = CARTESIAN_POINT('',(10.2935533906,31.7221825407,-19.7)) ;
#6109 = CARTESIAN_POINT('Origin',(8.91573593129,33.5242640687,-19.4)) ;
#6110 = CARTESIAN_POINT('',(8.70360389693,33.3121320344,-19.7)) ;
#6111 = CARTESIAN_POINT('Origin',(8.49147186258,33.1,-18.9999999999991)) ;
#6112 = CARTESIAN_POINT('',(8.49147186258,33.4,-19.7)) ;
#6113 = CARTESIAN_POINT('Origin',(-63.,33.7,-19.4)) ;
#6114 = CARTESIAN_POINT('',(-8.49147186258,33.4,-19.7)) ;
#6115 = CARTESIAN_POINT('Origin',(-8.49147186258,33.1,-18.9999999999991)) ;
#6116 = CARTESIAN_POINT('',(-8.70360389693,33.3121320344,-19.7)) ;
#6117 = CARTESIAN_POINT('Origin',(-1.79573593129,40.6442640687,-19.4)) ;
#6118 = CARTESIAN_POINT('',(-10.2935533906,31.7221825407,-19.7)) ;
#6119 = CARTESIAN_POINT('Origin',(-11.0713708499,32.5,-19.6000000000009)) ;
#6120 = CARTESIAN_POINT('',(-11.0713707703,31.4,-19.7)) ;
#6121 = CARTESIAN_POINT('Origin',(-63.,31.7,-19.4)) ;
#6122 = CARTESIAN_POINT('',(-22.6686291501,31.4,-19.7)) ;
#6123 = CARTESIAN_POINT('Origin',(-22.6686291501,32.5,-19.6000000000009)) ;
#6124 = CARTESIAN_POINT('',(-23.4464465531,31.7221824844,-19.7)) ;
#6125 = CARTESIAN_POINT('Origin',(13.6957359313,-4.99573593129,-19.4)) ;
#6126 = CARTESIAN_POINT('',(-25.0363961031,33.3121320344,-19.7)) ;
#6127 = CARTESIAN_POINT('Origin',(-25.2485281374,33.1,-18.9999999999991)) ;
#6128 = CARTESIAN_POINT('',(-25.2485281374,33.4,-19.7)) ;
#6129 = CARTESIAN_POINT('Origin',(-63.,33.7,-19.4)) ;
#6130 = CARTESIAN_POINT('',(-42.7514718626,33.4,-19.7)) ;
#6131 = CARTESIAN_POINT('Origin',(-42.7514718626,33.1,-18.9999999999991)) ;
#6132 = CARTESIAN_POINT('',(-42.9636038969,33.3121320344,-19.7)) ;
#6133 = CARTESIAN_POINT('Origin',(-36.0557359313,40.6442640687,-19.4)) ;
#6134 = CARTESIAN_POINT('',(-44.6121320344,31.6636038969,-19.7)) ;
#6135 = CARTESIAN_POINT('Origin',(-44.4,31.4514718626,-18.9999999999991)) ;
#6136 = CARTESIAN_POINT('',(-44.7,31.4514718626,-19.7)) ;
#6137 = CARTESIAN_POINT('Origin',(-45.,-5.42,-19.4)) ;
#6138 = CARTESIAN_POINT('',(-44.7,16.4985281374,-19.7)) ;
#6139 = CARTESIAN_POINT('Origin',(-44.4,16.4985281374,-18.9999999999991)) ;
#6140 = CARTESIAN_POINT('',(-44.6121320344,16.2863961031,-19.7)) ;
#6141 = CARTESIAN_POINT('Origin',(-22.9057359313,-5.84426406871,-19.4)) ;
#6142 = CARTESIAN_POINT('',(-42.4721825407,14.1464466094,-19.7)) ;
#6143 = CARTESIAN_POINT('Origin',(-43.25,13.3686291501,-19.6000000000009)) ;
#6144 = CARTESIAN_POINT('',(-42.15,13.3686292297,-19.7)) ;
#6145 = CARTESIAN_POINT('Origin',(-42.45,-5.42,-19.4)) ;
#6146 = CARTESIAN_POINT('Origin',(42.45,-5.42,-19.4)) ;
#6147 = CARTESIAN_POINT('',(0.,0.,0.)) ;
#6148 = CARTESIAN_POINT('Origin',(-1.46549439250795E-13,2.15383266777693E-13,
7.4999999999991)) ;
#6149 = CARTESIAN_POINT('',(-28.4431010968,-1.8,-20.)) ;
#6150 = CARTESIAN_POINT('',(-27.4410276775,-1.8,-19.)) ;
#6151 = CARTESIAN_POINT('Ctrl Pts',(-27.4410276775,-1.8,-19.)) ;
#6152 = CARTESIAN_POINT('Ctrl Pts',(-27.7749094354,-1.8,-19.3331657657)) ;
#6153 = CARTESIAN_POINT('Ctrl Pts',(-28.108944209,-1.8,-19.6665102407)) ;
#6154 = CARTESIAN_POINT('Ctrl Pts',(-28.4431010968,-1.8,-20.)) ;
#6155 = CARTESIAN_POINT('',(27.4410276775,-1.8,-19.)) ;
#6156 = CARTESIAN_POINT('Origin',(-5.3290705182E-15,3.5527136788E-15,-19.)) ;
#6157 = CARTESIAN_POINT('',(28.4431010968,-1.8,-20.)) ;
#6158 = CARTESIAN_POINT('Ctrl Pts',(27.4410276775,-1.8,-19.)) ;
#6159 = CARTESIAN_POINT('Ctrl Pts',(27.7749094354,-1.8,-19.3331657657)) ;
#6160 = CARTESIAN_POINT('Ctrl Pts',(28.108944209,-1.8,-19.6665102407)) ;
#6161 = CARTESIAN_POINT('Ctrl Pts',(28.4431010968,-1.8,-20.)) ;
#6162 = CARTESIAN_POINT('Origin',(-1.28742099732E-27,-4.4408920985E-15,-20.)) ;
#6163 = CARTESIAN_POINT('Origin',(0.,0.,0.)) ;
#6164 = CARTESIAN_POINT('',(-27.4410276775,-1.8,19.)) ;
#6165 = CARTESIAN_POINT('',(-27.4410276775,-1.8,0.)) ;
#6166 = CARTESIAN_POINT('',(27.4410276775,-1.8,19.)) ;
#6167 = CARTESIAN_POINT('Origin',(0.,0.,19.)) ;
#6168 = CARTESIAN_POINT('',(27.4410276775,-1.8,0.)) ;
#6169 = CARTESIAN_POINT('Origin',(-1.46549439250795E-13,2.15383266777693E-13,
-7.4999999999991)) ;
#6170 = CARTESIAN_POINT('',(28.4431010968,-1.8,20.)) ;
#6171 = CARTESIAN_POINT('',(-28.4431010968,-1.8,20.)) ;
#6172 = CARTESIAN_POINT('Origin',(-1.28742099732E-27,-4.4408920985E-15,20.)) ;
#6173 = CARTESIAN_POINT('Ctrl Pts',(27.4410276775,-1.8,19.)) ;
#6174 = CARTESIAN_POINT('Ctrl Pts',(27.7749094354,-1.8,19.3331657657)) ;
#6175 = CARTESIAN_POINT('Ctrl Pts',(28.108944209,-1.8,19.6665102407)) ;
#6176 = CARTESIAN_POINT('Ctrl Pts',(28.4431010968,-1.8,20.)) ;
#6177 = CARTESIAN_POINT('Ctrl Pts',(-27.4410276775,-1.8,19.)) ;
#6178 = CARTESIAN_POINT('Ctrl Pts',(-27.7749094354,-1.8,19.3331657657)) ;
#6179 = CARTESIAN_POINT('Ctrl Pts',(-28.108944209,-1.8,19.6665102407)) ;
#6180 = CARTESIAN_POINT('Ctrl Pts',(-28.4431010968,-1.8,20.)) ;
#6181 = CARTESIAN_POINT('Origin',(0.,0.,20.)) ;
#6182 = CARTESIAN_POINT('',(41.85,-1.8,20.)) ;
#6183 = CARTESIAN_POINT('',(35.1465505484,-1.8,20.)) ;
#6184 = CARTESIAN_POINT('',(-41.85,-1.8,20.)) ;
#6185 = CARTESIAN_POINT('',(-35.1465505484,-1.8,20.)) ;
#6186 = CARTESIAN_POINT('',(-41.85,-18.3699999990914,20.)) ;
#6187 = CARTESIAN_POINT('',(-41.85,-10.085,20.)) ;
#6188 = CARTESIAN_POINT('',(-41.82,-18.4,20.)) ;
#6189 = CARTESIAN_POINT('Origin',(-41.82,-18.37,20.)) ;
#6190 = CARTESIAN_POINT('',(-27.8642135633724,-18.4,20.)) ;
#6191 = CARTESIAN_POINT('',(-34.8421067812,-18.4,20.)) ;
#6192 = CARTESIAN_POINT('',(-26.7328427125,-18.8686291501,20.)) ;
#6193 = CARTESIAN_POINT('Origin',(-27.8642135624,-20.,20.)) ;
#6194 = CARTESIAN_POINT('',(-13.2186291495519,-32.382842713025,20.0000000000016)) ;
#6195 = CARTESIAN_POINT('',(-19.9757359313,-25.6257359313,20.)) ;
#6196 = CARTESIAN_POINT('',(-12.9357864376,-32.5,20.)) ;
#6197 = CARTESIAN_POINT('Origin',(-12.9357864376,-32.1,20.)) ;
#6198 = CARTESIAN_POINT('',(12.9357864376,-32.5,20.)) ;
#6199 = CARTESIAN_POINT('',(1.7763568394E-14,-32.5,20.)) ;
#6200 = CARTESIAN_POINT('',(13.2186291507794,-32.3828427117976,20.0000000000016)) ;
#6201 = CARTESIAN_POINT('Origin',(12.9357864376,-32.1,20.)) ;
#6202 = CARTESIAN_POINT('',(26.7328427125,-18.8686291501,20.)) ;
#6203 = CARTESIAN_POINT('',(19.9757359313,-25.6257359313,20.)) ;
#6204 = CARTESIAN_POINT('',(27.8642135616524,-18.4,20.)) ;
#6205 = CARTESIAN_POINT('Origin',(27.8642135624,-20.,20.)) ;
#6206 = CARTESIAN_POINT('',(41.82,-18.4,20.)) ;
#6207 = CARTESIAN_POINT('',(34.8421067812,-18.4,20.)) ;
#6208 = CARTESIAN_POINT('',(41.85,-18.3699999993067,20.)) ;
#6209 = CARTESIAN_POINT('Origin',(41.82,-18.37,20.)) ;
#6210 = CARTESIAN_POINT('',(41.85,-10.085,20.)) ;
#6211 = CARTESIAN_POINT('Origin',(-41.82,-18.37,19.0299999999991)) ;
#6212 = CARTESIAN_POINT('',(-42.45,-18.37,19.4)) ;
#6213 = CARTESIAN_POINT('',(-42.15,-18.37,19.7)) ;
#6214 = CARTESIAN_POINT('',(-41.82,-19.,19.4)) ;
#6215 = CARTESIAN_POINT('Origin',(-41.82,-18.37,19.4)) ;
#6216 = CARTESIAN_POINT('',(-41.82,-18.7,19.7)) ;
#6217 = CARTESIAN_POINT('Origin',(59.43,-19.,19.4)) ;
#6218 = CARTESIAN_POINT('',(-27.8642135624,-19.,19.4)) ;
#6219 = CARTESIAN_POINT('',(0.,-19.,19.4)) ;
#6220 = CARTESIAN_POINT('',(-27.8642135624,-18.7,19.7)) ;
#6221 = CARTESIAN_POINT('Origin',(-27.8642135624,-20.,19.4000000000009)) ;
#6222 = CARTESIAN_POINT('',(-27.1571067812,-19.2928932188,19.4)) ;
#6223 = CARTESIAN_POINT('Origin',(-27.8642135624,-20.,19.4)) ;
#6224 = CARTESIAN_POINT('',(-26.9449747468,-19.0807611845,19.7)) ;
#6225 = CARTESIAN_POINT('Origin',(-13.6428932188,-32.8071067812,19.4)) ;
#6226 = CARTESIAN_POINT('',(-13.6428932188,-32.8071067812,19.4)) ;
#6227 = CARTESIAN_POINT('',(-32.0643145751,-14.3856854249,19.4)) ;
#6228 = CARTESIAN_POINT('',(-13.4307611845,-32.5949747468,19.7)) ;
#6229 = CARTESIAN_POINT('Origin',(-12.9357864376,-32.1,19.3999999999991)) ;
#6230 = CARTESIAN_POINT('',(-12.9357864376,-33.1,19.4)) ;
#6231 = CARTESIAN_POINT('Origin',(-12.9357864376,-32.1,19.4)) ;
#6232 = CARTESIAN_POINT('',(-12.9357864376,-32.8,19.7)) ;
#6233 = CARTESIAN_POINT('Origin',(59.43,-33.1,19.4)) ;
#6234 = CARTESIAN_POINT('',(12.9357864376,-33.1,19.4)) ;
#6235 = CARTESIAN_POINT('',(0.,-33.1,19.4)) ;
#6236 = CARTESIAN_POINT('',(12.9357864376,-32.8,19.7)) ;
#6237 = CARTESIAN_POINT('Origin',(12.9357864376,-32.1,19.3999999999991)) ;
#6238 = CARTESIAN_POINT('',(13.6428932188,-32.8071067812,19.4)) ;
#6239 = CARTESIAN_POINT('Origin',(12.9357864376,-32.1,19.4)) ;
#6240 = CARTESIAN_POINT('',(13.4307611845,-32.5949747468,19.7)) ;
#6241 = CARTESIAN_POINT('Origin',(6.66573593129,-39.7842640687,19.4)) ;
#6242 = CARTESIAN_POINT('',(27.1571067812,-19.2928932188,19.4)) ;
#6243 = CARTESIAN_POINT('',(28.5757359313,-17.8742640687,19.4)) ;
#6244 = CARTESIAN_POINT('',(26.9449747468,-19.0807611845,19.7)) ;
#6245 = CARTESIAN_POINT('Origin',(27.8642135624,-20.,19.4000000000009)) ;
#6246 = CARTESIAN_POINT('',(27.8642135624,-19.,19.4)) ;
#6247 = CARTESIAN_POINT('Origin',(27.8642135624,-20.,19.4)) ;
#6248 = CARTESIAN_POINT('',(27.8642135624,-18.7,19.7)) ;
#6249 = CARTESIAN_POINT('Origin',(59.43,-19.,19.4)) ;
#6250 = CARTESIAN_POINT('',(41.82,-19.,19.4)) ;
#6251 = CARTESIAN_POINT('',(43.6471067812,-19.,19.4)) ;
#6252 = CARTESIAN_POINT('',(41.82,-18.7,19.7)) ;
#6253 = CARTESIAN_POINT('Origin',(41.82,-18.37,19.0299999999991)) ;
#6254 = CARTESIAN_POINT('',(42.45,-18.37,19.4)) ;
#6255 = CARTESIAN_POINT('Origin',(41.82,-18.37,19.4)) ;
#6256 = CARTESIAN_POINT('',(42.15,-18.37,19.7)) ;
#6257 = CARTESIAN_POINT('Origin',(42.45,-39.36,19.4)) ;
#6258 = CARTESIAN_POINT('',(42.45,-1.8,19.4)) ;
#6259 = CARTESIAN_POINT('',(42.45,-17.45,19.4)) ;
#6260 = CARTESIAN_POINT('',(42.15,-1.8,19.7)) ;
#6261 = CARTESIAN_POINT('Origin',(-42.45,-39.36,19.4)) ;
#6262 = CARTESIAN_POINT('',(-42.45,-1.8,19.4)) ;
#6263 = CARTESIAN_POINT('',(-42.15,-1.8,19.7)) ;
#6264 = CARTESIAN_POINT('',(-42.45,-17.45,19.4)) ;
#6265 = CARTESIAN_POINT('Origin',(0.,0.,-20.)) ;
#6266 = CARTESIAN_POINT('',(41.85,-18.3699989753,-20.)) ;
#6267 = CARTESIAN_POINT('',(41.85,-1.8,-20.)) ;
#6268 = CARTESIAN_POINT('',(41.85,-10.085,-20.)) ;
#6269 = CARTESIAN_POINT('',(41.82,-18.4,-20.)) ;
#6270 = CARTESIAN_POINT('Origin',(41.82,-18.37,-20.)) ;
#6271 = CARTESIAN_POINT('',(27.8642134654,-18.4,-20.)) ;
#6272 = CARTESIAN_POINT('',(34.8421067812,-18.4,-20.)) ;
#6273 = CARTESIAN_POINT('',(26.7328427125,-18.8686291501,-20.)) ;
#6274 = CARTESIAN_POINT('Origin',(27.8642135624,-20.,-20.)) ;
#6275 = CARTESIAN_POINT('',(13.2186291611,-32.3828427015,-20.)) ;
#6276 = CARTESIAN_POINT('',(19.9757359313,-25.6257359313,-20.)) ;
#6277 = CARTESIAN_POINT('',(12.9357864376,-32.5,-20.)) ;
#6278 = CARTESIAN_POINT('Origin',(12.9357864376,-32.1,-20.)) ;
#6279 = CARTESIAN_POINT('',(-12.9357864376,-32.5,-20.)) ;
#6280 = CARTESIAN_POINT('',(2.6645352591E-14,-32.5,-20.)) ;
#6281 = CARTESIAN_POINT('',(-13.2186291495519,-32.382842713025,-20.0000000000016)) ;
#6282 = CARTESIAN_POINT('Origin',(-12.9357864376,-32.1,-20.)) ;
#6283 = CARTESIAN_POINT('',(-26.7328427125,-18.8686291501,-20.)) ;
#6284 = CARTESIAN_POINT('',(-19.9757359313,-25.6257359313,-20.)) ;
#6285 = CARTESIAN_POINT('',(-27.8642135633724,-18.4,-20.)) ;
#6286 = CARTESIAN_POINT('Origin',(-27.8642135624,-20.,-20.)) ;
#6287 = CARTESIAN_POINT('',(-41.82,-18.4,-20.)) ;
#6288 = CARTESIAN_POINT('',(-34.8421067812,-18.4,-20.)) ;
#6289 = CARTESIAN_POINT('',(-41.85,-18.3699991048,-20.)) ;
#6290 = CARTESIAN_POINT('Origin',(-41.82,-18.37,-20.)) ;
#6291 = CARTESIAN_POINT('',(-41.85,-1.8,-20.)) ;
#6292 = CARTESIAN_POINT('',(-41.85,-10.085,-20.)) ;
#6293 = CARTESIAN_POINT('',(-35.1465505484,-1.8,-20.)) ;
#6294 = CARTESIAN_POINT('',(35.1465505484,-1.8,-20.)) ;
#6295 = CARTESIAN_POINT('Origin',(27.8642135624,-20.,0.)) ;
#6296 = CARTESIAN_POINT('',(27.1571067812,-19.2928932188,-19.4)) ;
#6297 = CARTESIAN_POINT('',(27.8642135323302,-19.,-19.4)) ;
#6298 = CARTESIAN_POINT('Origin',(27.8642135624,-20.,-19.4)) ;
#6299 = CARTESIAN_POINT('',(27.8642135624,-19.,0.)) ;
#6300 = CARTESIAN_POINT('',(27.1571067812,-19.2928932188,0.)) ;
#6301 = CARTESIAN_POINT('Origin',(-12.9357864376,-32.1,0.)) ;
#6302 = CARTESIAN_POINT('',(-12.9357864376,-33.1,-19.4)) ;
#6303 = CARTESIAN_POINT('',(-12.9357864376,-33.1,0.)) ;
#6304 = CARTESIAN_POINT('',(-13.6428932188,-32.8071067812,-19.4)) ;
#6305 = CARTESIAN_POINT('',(-13.6428932188,-32.8071067812,0.)) ;
#6306 = CARTESIAN_POINT('Origin',(-12.9357864376,-32.1,-19.4)) ;
#6307 = CARTESIAN_POINT('Origin',(-27.45,-19.,0.)) ;
#6308 = CARTESIAN_POINT('',(-27.1571067812,-19.2928932188,-19.4)) ;
#6309 = CARTESIAN_POINT('',(-27.1571067812,-19.2928932188,0.)) ;
#6310 = CARTESIAN_POINT('',(-20.4,-26.05,-19.4)) ;
#6311 = CARTESIAN_POINT('Origin',(27.45,-19.,0.)) ;
#6312 = CARTESIAN_POINT('',(13.6428932324447,-32.8071067675488,-19.4000000000025)) ;
#6313 = CARTESIAN_POINT('',(20.4,-26.05,-19.4)) ;
#6314 = CARTESIAN_POINT('',(13.6428932188,-32.8071067812,0.)) ;
#6315 = CARTESIAN_POINT('Origin',(12.9357864376,-32.1,0.)) ;
#6316 = CARTESIAN_POINT('',(12.9357864376,-33.1,-19.4)) ;
#6317 = CARTESIAN_POINT('',(12.9357864376,-33.1,0.)) ;
#6318 = CARTESIAN_POINT('Origin',(12.9357864376,-32.1,-19.4)) ;
#6319 = CARTESIAN_POINT('Origin',(-13.35,-33.1,0.)) ;
#6320 = CARTESIAN_POINT('',(1.06581410364E-14,-33.1,-19.4)) ;
#6321 = CARTESIAN_POINT('Origin',(-27.8642135624,-20.,0.)) ;
#6322 = CARTESIAN_POINT('',(-27.8642135624,-19.,-19.4)) ;
#6323 = CARTESIAN_POINT('Origin',(-27.8642135624,-20.,-19.4)) ;
#6324 = CARTESIAN_POINT('',(-27.8642135624,-19.,0.)) ;
#6325 = CARTESIAN_POINT('Origin',(-27.4410276775,-1.8,0.)) ;
#6326 = CARTESIAN_POINT('',(42.45,-1.8,-19.4)) ;
#6327 = CARTESIAN_POINT('',(42.45,-1.8,0.)) ;
#6328 = CARTESIAN_POINT('',(42.15,-1.8,-19.7)) ;
#6329 = CARTESIAN_POINT('',(32.1478566738563,-1.8,11.5581330004637)) ;
#6330 = CARTESIAN_POINT('Origin',(35.,-1.8,10.)) ;
#6331 = CARTESIAN_POINT('',(32.1478566738563,-1.8,-8.44186699953634)) ;
#6332 = CARTESIAN_POINT('Origin',(35.,-1.8,-10.)) ;
#6333 = CARTESIAN_POINT('Origin',(-27.4410276775,-1.8,0.)) ;
#6334 = CARTESIAN_POINT('',(-42.45,-1.8,-19.4)) ;
#6335 = CARTESIAN_POINT('',(-42.45,-1.8,0.)) ;
#6336 = CARTESIAN_POINT('',(-42.15,-1.8,-19.7)) ;
#6337 = CARTESIAN_POINT('',(-37.8521433261437,-1.8,-8.44186699953634)) ;
#6338 = CARTESIAN_POINT('Origin',(-35.,-1.8,-10.)) ;
#6339 = CARTESIAN_POINT('',(-37.8521433261437,-1.8,11.5581330004637)) ;
#6340 = CARTESIAN_POINT('Origin',(-35.,-1.8,10.)) ;
#6341 = CARTESIAN_POINT('Origin',(42.45,-1.8,0.)) ;
#6342 = CARTESIAN_POINT('',(42.449999999864,-18.3699892404226,-19.4000000000257)) ;
#6343 = CARTESIAN_POINT('',(42.45,-10.085,-19.4)) ;
#6344 = CARTESIAN_POINT('',(42.45,-18.37,0.)) ;
#6345 = CARTESIAN_POINT('Origin',(41.82,-18.37,0.)) ;
#6346 = CARTESIAN_POINT('',(41.82,-19.,-19.4)) ;
#6347 = CARTESIAN_POINT('',(41.82,-19.,0.)) ;
#6348 = CARTESIAN_POINT('Origin',(41.82,-18.37,-19.4)) ;
#6349 = CARTESIAN_POINT('Origin',(-42.45,-1.8,0.)) ;
#6350 = CARTESIAN_POINT('',(-42.4499999999024,-18.3699906000849,-19.4000000000289)) ;
#6351 = CARTESIAN_POINT('',(-42.45,-18.37,0.)) ;
#6352 = CARTESIAN_POINT('',(-42.45,-10.085,-19.4)) ;
#6353 = CARTESIAN_POINT('Origin',(-41.82,-18.37,0.)) ;
#6354 = CARTESIAN_POINT('',(-41.82,-19.,-19.4)) ;
#6355 = CARTESIAN_POINT('',(-41.82,-19.,0.)) ;
#6356 = CARTESIAN_POINT('Origin',(-41.82,-18.37,-19.4)) ;
#6357 = CARTESIAN_POINT('Origin',(-41.82,-18.37,-19.0299999999991)) ;
#6358 = CARTESIAN_POINT('',(-42.1499999999,-18.3699901523,-19.7)) ;
#6359 = CARTESIAN_POINT('',(-41.82,-18.7,-19.7)) ;
#6360 = CARTESIAN_POINT('Origin',(59.43,-19.,-19.4)) ;
#6361 = CARTESIAN_POINT('',(-27.8642135624,-18.7,-19.7)) ;
#6362 = CARTESIAN_POINT('',(7.1054273576E-15,-19.,-19.4)) ;
#6363 = CARTESIAN_POINT('Origin',(-27.8642135624,-20.,-19.4000000000009)) ;
#6364 = CARTESIAN_POINT('',(-26.9449747468,-19.0807611845,-19.7)) ;
#6365 = CARTESIAN_POINT('Origin',(-6.66573593129,-39.7842640687,-19.4)) ;
#6366 = CARTESIAN_POINT('',(-13.4307611845,-32.5949747468,-19.7)) ;
#6367 = CARTESIAN_POINT('Origin',(-12.9357864376,-32.1,-19.3999999999991)) ;
#6368 = CARTESIAN_POINT('',(-12.9357864376,-32.8,-19.7)) ;
#6369 = CARTESIAN_POINT('Origin',(59.43,-33.1,-19.4)) ;
#6370 = CARTESIAN_POINT('',(12.9357864376,-32.8,-19.7)) ;
#6371 = CARTESIAN_POINT('Origin',(12.9357864376,-32.1,-19.3999999999991)) ;
#6372 = CARTESIAN_POINT('',(13.4307612037,-32.5949747276,-19.7)) ;
#6373 = CARTESIAN_POINT('Origin',(6.66573593129,-39.7842640687,-19.4)) ;
#6374 = CARTESIAN_POINT('',(26.9449747468,-19.0807611845,-19.7)) ;
#6375 = CARTESIAN_POINT('Origin',(27.8642135624,-20.,-19.4000000000009)) ;
#6376 = CARTESIAN_POINT('',(27.8642134836,-18.7,-19.7)) ;
#6377 = CARTESIAN_POINT('Origin',(59.43,-19.,-19.4)) ;
#6378 = CARTESIAN_POINT('',(41.82,-18.7,-19.7)) ;
#6379 = CARTESIAN_POINT('',(43.6471067812,-19.,-19.4)) ;
#6380 = CARTESIAN_POINT('Origin',(41.82,-18.37,-19.0299999999991)) ;
#6381 = CARTESIAN_POINT('',(42.1499999998,-18.3699887279,-19.7)) ;
#6382 = CARTESIAN_POINT('Origin',(42.45,-39.36,-19.4)) ;
#6383 = CARTESIAN_POINT('Origin',(-42.45,-39.36,-19.4)) ;
#6384 = CARTESIAN_POINT('Origin',(-35.,-18.9,10.)) ;
#6385 = CARTESIAN_POINT('',(-32.3636514836019,-18.4999999999988,8.09942995391034)) ;
#6386 = CARTESIAN_POINT('',(-37.8521433261437,-18.5,11.5581330004637)) ;
#6387 = CARTESIAN_POINT('Origin',(-35.,-18.5,10.)) ;
#6388 = CARTESIAN_POINT('',(-37.8521433261437,-18.9,11.5581330004637)) ;
#6389 = CARTESIAN_POINT('Origin',(-35.,-18.5,10.)) ;
#6390 = CARTESIAN_POINT('Origin',(-35.,-16.2499999999989,10.0000000000003)) ;
#6391 = CARTESIAN_POINT('',(-31.9580594041556,-18.9999999999991,7.80703456220392)) ;
#6392 = CARTESIAN_POINT('',(-34.1888158411087,-16.2499999999991,9.4152092165881)) ;
#6393 = CARTESIAN_POINT('Origin',(-35.,-19.,10.)) ;
#6394 = CARTESIAN_POINT('Origin',(-35.,-18.9,-10.)) ;
#6395 = CARTESIAN_POINT('',(-32.363651483595,-18.4999999999987,-11.9005700460802)) ;
#6396 = CARTESIAN_POINT('',(-37.8521433261437,-18.5,-8.44186699953634)) ;
#6397 = CARTESIAN_POINT('Origin',(-35.,-18.5,-10.)) ;
#6398 = CARTESIAN_POINT('',(-37.8521433261437,-18.9,-8.44186699953634)) ;
#6399 = CARTESIAN_POINT('Origin',(-35.,-18.5,-10.)) ;
#6400 = CARTESIAN_POINT('Origin',(-42.45,-19.,0.)) ;
#6401 = CARTESIAN_POINT('',(-31.958059404148,-18.9999999999985,-12.1929654377848)) ;
#6402 = CARTESIAN_POINT('Origin',(-35.,-19.,-10.)) ;
#6403 = CARTESIAN_POINT('Origin',(-35.,-16.2499999999989,-9.99999999999968)) ;
#6404 = CARTESIAN_POINT('',(-34.1888158411066,-16.2499999999991,-10.584790783409)) ;
#6405 = CARTESIAN_POINT('Origin',(35.,-18.9,-10.)) ;
#6406 = CARTESIAN_POINT('',(37.6363485163993,-18.4999999999987,-11.9005700460881)) ;
#6407 = CARTESIAN_POINT('',(32.1478566738563,-18.5,-8.44186699953634)) ;
#6408 = CARTESIAN_POINT('Origin',(35.,-18.5,-10.)) ;
#6409 = CARTESIAN_POINT('',(32.1478566738563,-18.9,-8.44186699953634)) ;
#6410 = CARTESIAN_POINT('Origin',(35.,-18.5,-10.)) ;
#6411 = CARTESIAN_POINT('Origin',(35.,-16.2499999999989,-9.99999999999968)) ;
#6412 = CARTESIAN_POINT('',(38.0419405958458,-18.9999999999991,-12.1929654377943)) ;
#6413 = CARTESIAN_POINT('',(35.8111841588916,-16.2499999999991,-10.5847907834114)) ;
#6414 = CARTESIAN_POINT('Origin',(35.,-19.,-10.)) ;
#6415 = CARTESIAN_POINT('Origin',(35.,-18.9,10.)) ;
#6416 = CARTESIAN_POINT('',(37.6363485163777,-18.4999999999987,8.09942995388186)) ;
#6417 = CARTESIAN_POINT('',(32.1478566738563,-18.5,11.5581330004637)) ;
#6418 = CARTESIAN_POINT('Origin',(35.,-18.5,10.)) ;
#6419 = CARTESIAN_POINT('',(32.1478566738563,-18.9,11.5581330004637)) ;
#6420 = CARTESIAN_POINT('Origin',(35.,-18.5,10.)) ;
#6421 = CARTESIAN_POINT('Origin',(-42.45,-19.,0.)) ;
#6422 = CARTESIAN_POINT('',(38.0419405958204,-18.9999999999985,7.80703456217137)) ;
#6423 = CARTESIAN_POINT('Origin',(35.,-19.,10.)) ;
#6424 = CARTESIAN_POINT('Origin',(35.,-16.2499999999989,10.0000000000003)) ;
#6425 = CARTESIAN_POINT('',(35.811184158885,-16.2499999999991,9.41520921657933)) ;
#6426 = CARTESIAN_POINT('',(0.,0.,0.)) ;
#6427 = CARTESIAN_POINT('Origin',(-35.,-19.5,10.)) ;
#6428 = CARTESIAN_POINT('',(-41.,-20.,10.)) ;
#6429 = CARTESIAN_POINT('Origin',(-35.,-20.,10.)) ;
#6430 = CARTESIAN_POINT('',(-41.,-19.,10.)) ;
#6431 = CARTESIAN_POINT('',(-41.,-19.5,10.)) ;
#6432 = CARTESIAN_POINT('Origin',(-35.,-19.,10.)) ;
#6433 = CARTESIAN_POINT('Origin',(-35.,-19.5,10.)) ;
#6434 = CARTESIAN_POINT('',(-38.2,-19.,10.)) ;
#6435 = CARTESIAN_POINT('Origin',(-35.,-19.,10.)) ;
#6436 = CARTESIAN_POINT('',(-38.2,-20.,10.)) ;
#6437 = CARTESIAN_POINT('',(-38.2,-19.5,10.)) ;
#6438 = CARTESIAN_POINT('Origin',(-35.,-20.,10.)) ;
#6439 = CARTESIAN_POINT('Origin',(0.,-19.,0.)) ;
#6440 = CARTESIAN_POINT('Origin',(0.,-20.,0.)) ;
#6441 = CARTESIAN_POINT('',(0.,0.,0.)) ;
#6442 = CARTESIAN_POINT('Origin',(-35.,-19.5,-10.)) ;
#6443 = CARTESIAN_POINT('',(-41.,-20.,-10.)) ;
#6444 = CARTESIAN_POINT('Origin',(-35.,-20.,-10.)) ;
#6445 = CARTESIAN_POINT('',(-41.,-19.,-10.)) ;
#6446 = CARTESIAN_POINT('',(-41.,-19.5,-10.)) ;
#6447 = CARTESIAN_POINT('Origin',(-35.,-19.,-10.)) ;
#6448 = CARTESIAN_POINT('Origin',(-35.,-19.5,-10.)) ;
#6449 = CARTESIAN_POINT('',(-38.2,-19.,-10.)) ;
#6450 = CARTESIAN_POINT('Origin',(-35.,-19.,-10.)) ;
#6451 = CARTESIAN_POINT('',(-38.2,-20.,-10.)) ;
#6452 = CARTESIAN_POINT('',(-38.2,-19.5,-10.)) ;
#6453 = CARTESIAN_POINT('Origin',(-35.,-20.,-10.)) ;
#6454 = CARTESIAN_POINT('Origin',(0.,-19.,0.)) ;
#6455 = CARTESIAN_POINT('Origin',(0.,-20.,0.)) ;
#6456 = CARTESIAN_POINT('',(0.,0.,0.)) ;
#6457 = CARTESIAN_POINT('Origin',(35.,-19.5,10.)) ;
#6458 = CARTESIAN_POINT('',(29.,-20.,10.)) ;
#6459 = CARTESIAN_POINT('Origin',(35.,-20.,10.)) ;
#6460 = CARTESIAN_POINT('',(29.,-19.,10.)) ;
#6461 = CARTESIAN_POINT('',(29.,-19.5,10.)) ;
#6462 = CARTESIAN_POINT('Origin',(35.,-19.,10.)) ;
#6463 = CARTESIAN_POINT('Origin',(35.,-19.5,10.)) ;
#6464 = CARTESIAN_POINT('',(31.8,-19.,10.)) ;
#6465 = CARTESIAN_POINT('Origin',(35.,-19.,10.)) ;
#6466 = CARTESIAN_POINT('',(31.8,-20.,10.)) ;
#6467 = CARTESIAN_POINT('',(31.8,-19.5,10.)) ;
#6468 = CARTESIAN_POINT('Origin',(35.,-20.,10.)) ;
#6469 = CARTESIAN_POINT('Origin',(0.,-19.,0.)) ;
#6470 = CARTESIAN_POINT('Origin',(0.,-20.,0.)) ;
#6471 = CARTESIAN_POINT('',(0.,0.,0.)) ;
#6472 = CARTESIAN_POINT('Origin',(35.,-19.5,-10.)) ;
#6473 = CARTESIAN_POINT('',(29.,-20.,-10.)) ;
#6474 = CARTESIAN_POINT('Origin',(35.,-20.,-10.)) ;
#6475 = CARTESIAN_POINT('',(29.,-19.,-10.)) ;
#6476 = CARTESIAN_POINT('',(29.,-19.5,-10.)) ;
#6477 = CARTESIAN_POINT('Origin',(35.,-19.,-10.)) ;
#6478 = CARTESIAN_POINT('Origin',(35.,-19.5,-10.)) ;
#6479 = CARTESIAN_POINT('',(31.8,-19.,-10.)) ;
#6480 = CARTESIAN_POINT('Origin',(35.,-19.,-10.)) ;
#6481 = CARTESIAN_POINT('',(31.8,-20.,-10.)) ;
#6482 = CARTESIAN_POINT('',(31.8,-19.5,-10.)) ;
#6483 = CARTESIAN_POINT('Origin',(35.,-20.,-10.)) ;
#6484 = CARTESIAN_POINT('Origin',(0.,-19.,0.)) ;
#6485 = CARTESIAN_POINT('Origin',(0.,-20.,0.)) ;
#6486 = CARTESIAN_POINT('',(0.,0.,0.)) ;
#6487 = CARTESIAN_POINT('Origin',(-37.5,-26.,11.443375673)) ;
#6488 = CARTESIAN_POINT('',(-37.5,-26.,11.443375673)) ;
#6489 = CARTESIAN_POINT('',(-37.5,-23.,11.443375673)) ;
#6490 = CARTESIAN_POINT('',(-37.5,-24.5,11.443375673)) ;
#6491 = CARTESIAN_POINT('',(-37.5,-26.,8.55662432703)) ;
#6492 = CARTESIAN_POINT('',(-37.5,-26.,10.)) ;
#6493 = CARTESIAN_POINT('',(-37.5,-23.,8.55662432703)) ;
#6494 = CARTESIAN_POINT('',(-37.5,-24.5,8.55662432703)) ;
#6495 = CARTESIAN_POINT('',(-37.5,-23.,10.)) ;
#6496 = CARTESIAN_POINT('Origin',(-35.,-26.,12.8867513459)) ;
#6497 = CARTESIAN_POINT('',(-35.,-26.,12.8867513459)) ;
#6498 = CARTESIAN_POINT('',(-35.,-23.,12.8867513459)) ;
#6499 = CARTESIAN_POINT('',(-35.,-24.5,12.8867513459)) ;
#6500 = CARTESIAN_POINT('',(-36.25,-26.,12.1650635095)) ;
#6501 = CARTESIAN_POINT('',(-36.25,-23.,12.1650635095)) ;
#6502 = CARTESIAN_POINT('Origin',(-37.5,-26.,8.55662432703)) ;
#6503 = CARTESIAN_POINT('',(-35.,-26.,7.11324865405)) ;
#6504 = CARTESIAN_POINT('',(-36.25,-26.,7.83493649054)) ;
#6505 = CARTESIAN_POINT('',(-35.,-23.,7.11324865405)) ;
#6506 = CARTESIAN_POINT('',(-35.,-24.5,7.11324865405)) ;
#6507 = CARTESIAN_POINT('',(-36.25,-23.,7.83493649054)) ;
#6508 = CARTESIAN_POINT('Origin',(-35.,-23.,10.)) ;
#6509 = CARTESIAN_POINT('',(-32.5,-23.,8.55662432703)) ;
#6510 = CARTESIAN_POINT('',(-33.75,-23.,7.83493649054)) ;
#6511 = CARTESIAN_POINT('',(-32.5,-23.,11.443375673)) ;
#6512 = CARTESIAN_POINT('',(-32.5,-23.,10.)) ;
#6513 = CARTESIAN_POINT('',(-33.75,-23.,12.1650635095)) ;
#6514 = CARTESIAN_POINT('Origin',(-32.5,-26.,11.443375673)) ;
#6515 = CARTESIAN_POINT('',(-32.5,-26.,11.443375673)) ;
#6516 = CARTESIAN_POINT('',(-32.5,-24.5,11.443375673)) ;
#6517 = CARTESIAN_POINT('',(-33.75,-26.,12.1650635095)) ;
#6518 = CARTESIAN_POINT('Origin',(-35.,-26.,7.11324865405)) ;
#6519 = CARTESIAN_POINT('',(-32.5,-26.,8.55662432703)) ;
#6520 = CARTESIAN_POINT('',(-33.75,-26.,7.83493649054)) ;
#6521 = CARTESIAN_POINT('',(-32.5,-24.5,8.55662432703)) ;
#6522 = CARTESIAN_POINT('Origin',(-32.5,-26.,8.55662432703)) ;
#6523 = CARTESIAN_POINT('',(-32.5,-26.,10.)) ;
#6524 = CARTESIAN_POINT('Origin',(-35.,-26.,10.)) ;
#6525 = CARTESIAN_POINT('',(-37.1094723699,-26.,13.8613632723)) ;
#6526 = CARTESIAN_POINT('Origin',(-35.,-26.,10.)) ;
#6527 = CARTESIAN_POINT('Origin',(-35.,-20.,5.)) ;
#6528 = CARTESIAN_POINT('',(-37.397127693,-20.,14.3879128095)) ;
#6529 = CARTESIAN_POINT('Origin',(-35.,-20.,10.)) ;
#6530 = CARTESIAN_POINT('',(-36.5581330005,-20.,12.8521433261)) ;
#6531 = CARTESIAN_POINT('Origin',(-35.,-20.,10.)) ;
#6532 = CARTESIAN_POINT('Origin',(-35.,40.,7.5)) ;
#6533 = CARTESIAN_POINT('',(-36.1985638465,40.,12.1939564047)) ;
#6534 = CARTESIAN_POINT('Origin',(-35.,40.,10.)) ;
#6535 = CARTESIAN_POINT('Origin',(-35.,-25.4,10.)) ;
#6536 = CARTESIAN_POINT('',(-37.397127693,-25.4,14.3879128095)) ;
#6537 = CARTESIAN_POINT('Origin',(-37.1094723698585,-25.4,13.8613632723176)) ;
#6538 = CARTESIAN_POINT('Origin',(-35.,-25.4,10.)) ;
#6539 = CARTESIAN_POINT('Origin',(-35.,7.,10.)) ;
#6540 = CARTESIAN_POINT('',(-37.397127693021,7.,14.3879128094519)) ;
#6541 = CARTESIAN_POINT('Origin',(-35.,-19.75,10.)) ;
#6542 = CARTESIAN_POINT('',(-36.4382766158,-19.75,12.6327476857)) ;
#6543 = CARTESIAN_POINT('Origin',(-36.5581330004637,-19.75,12.8521433261437)) ;
#6544 = CARTESIAN_POINT('Origin',(-35.,-19.75,10.)) ;
#6545 = CARTESIAN_POINT('Origin',(-35.,7.,10.)) ;
#6546 = CARTESIAN_POINT('',(-36.4382766158,39.5,12.6327476857)) ;
#6547 = CARTESIAN_POINT('',(-36.4382766158126,7.,12.6327476856711)) ;
#6548 = CARTESIAN_POINT('Origin',(-35.,39.5,10.)) ;
#6549 = CARTESIAN_POINT('Origin',(-35.,40.,10.)) ;
#6550 = CARTESIAN_POINT('',(-36.1985638465105,40.,12.1939564047259)) ;
#6551 = CARTESIAN_POINT('',(0.,0.,0.)) ;
#6552 = CARTESIAN_POINT('Origin',(-37.5,-26.,11.443375673)) ;
#6553 = CARTESIAN_POINT('',(-37.5,-26.,-8.55662432703)) ;
#6554 = CARTESIAN_POINT('',(-37.5,-23.,-8.55662432703)) ;
#6555 = CARTESIAN_POINT('',(-37.5,-24.5,-8.55662432703)) ;
#6556 = CARTESIAN_POINT('',(-37.5,-26.,-11.443375673)) ;
#6557 = CARTESIAN_POINT('',(-37.5,-26.,-10.)) ;
#6558 = CARTESIAN_POINT('',(-37.5,-23.,-11.443375673)) ;
#6559 = CARTESIAN_POINT('',(-37.5,-24.5,-11.443375673)) ;
#6560 = CARTESIAN_POINT('',(-37.5,-23.,-10.)) ;
#6561 = CARTESIAN_POINT('Origin',(-35.,-26.,-7.11324865405)) ;
#6562 = CARTESIAN_POINT('',(-35.,-26.,-7.11324865405)) ;
#6563 = CARTESIAN_POINT('',(-35.,-23.,-7.11324865405)) ;
#6564 = CARTESIAN_POINT('',(-35.,-24.5,-7.11324865405)) ;
#6565 = CARTESIAN_POINT('',(-36.25,-26.,-7.83493649054)) ;
#6566 = CARTESIAN_POINT('',(-36.25,-23.,-7.83493649054)) ;
#6567 = CARTESIAN_POINT('Origin',(-37.5,-26.,-11.443375673)) ;
#6568 = CARTESIAN_POINT('',(-35.,-26.,-12.8867513459)) ;
#6569 = CARTESIAN_POINT('',(-36.25,-26.,-12.1650635095)) ;
#6570 = CARTESIAN_POINT('',(-35.,-23.,-12.8867513459)) ;
#6571 = CARTESIAN_POINT('',(-35.,-24.5,-12.8867513459)) ;
#6572 = CARTESIAN_POINT('',(-36.25,-23.,-12.1650635095)) ;
#6573 = CARTESIAN_POINT('Origin',(-35.,-23.,10.)) ;
#6574 = CARTESIAN_POINT('',(-32.5,-23.,-11.443375673)) ;
#6575 = CARTESIAN_POINT('',(-33.75,-23.,-12.1650635095)) ;
#6576 = CARTESIAN_POINT('',(-32.5,-23.,-8.55662432703)) ;
#6577 = CARTESIAN_POINT('',(-32.5,-23.,-10.)) ;
#6578 = CARTESIAN_POINT('',(-33.75,-23.,-7.83493649054)) ;
#6579 = CARTESIAN_POINT('Origin',(-32.5,-26.,-8.55662432703)) ;
#6580 = CARTESIAN_POINT('',(-32.5,-26.,-8.55662432703)) ;
#6581 = CARTESIAN_POINT('',(-32.5,-24.5,-8.55662432703)) ;
#6582 = CARTESIAN_POINT('',(-33.75,-26.,-7.83493649054)) ;
#6583 = CARTESIAN_POINT('Origin',(-35.,-26.,-12.8867513459)) ;
#6584 = CARTESIAN_POINT('',(-32.5,-26.,-11.443375673)) ;
#6585 = CARTESIAN_POINT('',(-33.75,-26.,-12.1650635095)) ;
#6586 = CARTESIAN_POINT('',(-32.5,-24.5,-11.443375673)) ;
#6587 = CARTESIAN_POINT('Origin',(-32.5,-26.,8.55662432703)) ;
#6588 = CARTESIAN_POINT('',(-32.5,-26.,-10.)) ;
#6589 = CARTESIAN_POINT('Origin',(-35.,-26.,10.)) ;
#6590 = CARTESIAN_POINT('',(-37.1094723699,-26.,-6.13863672768)) ;
#6591 = CARTESIAN_POINT('Origin',(-35.,-26.,-10.)) ;
#6592 = CARTESIAN_POINT('Origin',(-35.,-20.,5.)) ;
#6593 = CARTESIAN_POINT('',(-37.397127693,-20.,-5.61208719055)) ;
#6594 = CARTESIAN_POINT('Origin',(-35.,-20.,-10.)) ;
#6595 = CARTESIAN_POINT('',(-36.5581330005,-20.,-7.14785667386)) ;
#6596 = CARTESIAN_POINT('Origin',(-35.,-20.,-10.)) ;
#6597 = CARTESIAN_POINT('Origin',(-35.,40.,7.5)) ;
#6598 = CARTESIAN_POINT('',(-36.1985638465,40.,-7.80604359527)) ;
#6599 = CARTESIAN_POINT('Origin',(-35.,40.,-10.)) ;
#6600 = CARTESIAN_POINT('Origin',(-35.,-25.4,-10.)) ;
#6601 = CARTESIAN_POINT('',(-37.397127693,-25.4,-5.61208719055)) ;
#6602 = CARTESIAN_POINT('Origin',(-37.1094723698585,-25.4,-6.13863672768236)) ;
#6603 = CARTESIAN_POINT('Origin',(-35.,-25.4,-10.)) ;
#6604 = CARTESIAN_POINT('Origin',(-35.,7.,-10.)) ;
#6605 = CARTESIAN_POINT('',(-37.397127693021,7.,-5.61208719054814)) ;
#6606 = CARTESIAN_POINT('Origin',(-35.,-19.75,-10.)) ;
#6607 = CARTESIAN_POINT('',(-36.4382766158,-19.75,-7.36725231433)) ;
#6608 = CARTESIAN_POINT('Origin',(-36.5581330004637,-19.75,-7.14785667385629)) ;
#6609 = CARTESIAN_POINT('Origin',(-35.,-19.75,-10.)) ;
#6610 = CARTESIAN_POINT('Origin',(-35.,7.,-10.)) ;
#6611 = CARTESIAN_POINT('',(-36.4382766158,39.5,-7.36725231433)) ;
#6612 = CARTESIAN_POINT('',(-36.4382766158126,7.,-7.36725231432888)) ;
#6613 = CARTESIAN_POINT('Origin',(-35.,39.5,-10.)) ;
#6614 = CARTESIAN_POINT('Origin',(-35.,40.,-10.)) ;
#6615 = CARTESIAN_POINT('',(-36.1985638465105,40.,-7.80604359527407)) ;
#6616 = CARTESIAN_POINT('',(0.,0.,0.)) ;
#6617 = CARTESIAN_POINT('Origin',(32.5,-26.,11.443375673)) ;
#6618 = CARTESIAN_POINT('',(32.5,-26.,11.443375673)) ;
#6619 = CARTESIAN_POINT('',(32.5,-23.,11.443375673)) ;
#6620 = CARTESIAN_POINT('',(32.5,-24.5,11.443375673)) ;
#6621 = CARTESIAN_POINT('',(32.5,-26.,8.55662432703)) ;
#6622 = CARTESIAN_POINT('',(32.5,-26.,10.)) ;
#6623 = CARTESIAN_POINT('',(32.5,-23.,8.55662432703)) ;
#6624 = CARTESIAN_POINT('',(32.5,-24.5,8.55662432703)) ;
#6625 = CARTESIAN_POINT('',(32.5,-23.,10.)) ;
#6626 = CARTESIAN_POINT('Origin',(35.,-26.,12.8867513459)) ;
#6627 = CARTESIAN_POINT('',(35.,-26.,12.8867513459)) ;
#6628 = CARTESIAN_POINT('',(35.,-23.,12.8867513459)) ;
#6629 = CARTESIAN_POINT('',(35.,-24.5,12.8867513459)) ;
#6630 = CARTESIAN_POINT('',(33.75,-26.,12.1650635095)) ;
#6631 = CARTESIAN_POINT('',(33.75,-23.,12.1650635095)) ;
#6632 = CARTESIAN_POINT('Origin',(32.5,-26.,8.55662432703)) ;
#6633 = CARTESIAN_POINT('',(35.,-26.,7.11324865405)) ;
#6634 = CARTESIAN_POINT('',(33.75,-26.,7.83493649054)) ;
#6635 = CARTESIAN_POINT('',(35.,-23.,7.11324865405)) ;
#6636 = CARTESIAN_POINT('',(35.,-24.5,7.11324865405)) ;
#6637 = CARTESIAN_POINT('',(33.75,-23.,7.83493649054)) ;
#6638 = CARTESIAN_POINT('Origin',(-35.,-23.,10.)) ;
#6639 = CARTESIAN_POINT('',(37.5,-23.,8.55662432703)) ;
#6640 = CARTESIAN_POINT('',(36.25,-23.,7.83493649054)) ;
#6641 = CARTESIAN_POINT('',(37.5,-23.,11.443375673)) ;
#6642 = CARTESIAN_POINT('',(37.5,-23.,10.)) ;
#6643 = CARTESIAN_POINT('',(36.25,-23.,12.1650635095)) ;
#6644 = CARTESIAN_POINT('Origin',(37.5,-26.,11.443375673)) ;
#6645 = CARTESIAN_POINT('',(37.5,-26.,11.443375673)) ;
#6646 = CARTESIAN_POINT('',(37.5,-24.5,11.443375673)) ;
#6647 = CARTESIAN_POINT('',(36.25,-26.,12.1650635095)) ;
#6648 = CARTESIAN_POINT('Origin',(35.,-26.,7.11324865405)) ;
#6649 = CARTESIAN_POINT('',(37.5,-26.,8.55662432703)) ;
#6650 = CARTESIAN_POINT('',(36.25,-26.,7.83493649054)) ;
#6651 = CARTESIAN_POINT('',(37.5,-24.5,8.55662432703)) ;
#6652 = CARTESIAN_POINT('Origin',(37.5,-26.,8.55662432703)) ;
#6653 = CARTESIAN_POINT('',(37.5,-26.,10.)) ;
#6654 = CARTESIAN_POINT('Origin',(-35.,-26.,10.)) ;
#6655 = CARTESIAN_POINT('',(32.8905276301,-26.,13.8613632723)) ;
#6656 = CARTESIAN_POINT('Origin',(35.,-26.,10.)) ;
#6657 = CARTESIAN_POINT('Origin',(-35.,-20.,5.)) ;
#6658 = CARTESIAN_POINT('',(32.602872307,-20.,14.3879128095)) ;
#6659 = CARTESIAN_POINT('Origin',(35.,-20.,10.)) ;
#6660 = CARTESIAN_POINT('',(33.4418669995,-20.,12.8521433261)) ;
#6661 = CARTESIAN_POINT('Origin',(35.,-20.,10.)) ;
#6662 = CARTESIAN_POINT('Origin',(-35.,40.,7.5)) ;
#6663 = CARTESIAN_POINT('',(33.8014361535,40.,12.1939564047)) ;
#6664 = CARTESIAN_POINT('Origin',(35.,40.,10.)) ;
#6665 = CARTESIAN_POINT('Origin',(35.,-25.4,10.)) ;
#6666 = CARTESIAN_POINT('',(32.602872307,-25.4,14.3879128095)) ;
#6667 = CARTESIAN_POINT('Origin',(32.8905276301415,-25.4,13.8613632723176)) ;
#6668 = CARTESIAN_POINT('Origin',(35.,-25.4,10.)) ;
#6669 = CARTESIAN_POINT('Origin',(35.,7.,10.)) ;
#6670 = CARTESIAN_POINT('',(32.602872306979,7.,14.3879128094519)) ;
#6671 = CARTESIAN_POINT('Origin',(35.,-19.75,10.)) ;
#6672 = CARTESIAN_POINT('',(33.5617233842,-19.75,12.6327476857)) ;
#6673 = CARTESIAN_POINT('Origin',(33.4418669995363,-19.75,12.8521433261437)) ;
#6674 = CARTESIAN_POINT('Origin',(35.,-19.75,10.)) ;
#6675 = CARTESIAN_POINT('Origin',(35.,7.,10.)) ;
#6676 = CARTESIAN_POINT('',(33.5617233842,39.5,12.6327476857)) ;
#6677 = CARTESIAN_POINT('',(33.5617233841874,7.,12.6327476856711)) ;
#6678 = CARTESIAN_POINT('Origin',(35.,39.5,10.)) ;
#6679 = CARTESIAN_POINT('Origin',(35.,40.,10.)) ;
#6680 = CARTESIAN_POINT('',(33.8014361534895,40.,12.1939564047259)) ;
#6681 = CARTESIAN_POINT('',(0.,0.,0.)) ;
#6682 = CARTESIAN_POINT('Origin',(32.5,-26.,-8.55662432703)) ;
#6683 = CARTESIAN_POINT('',(32.5,-26.,-8.55662432703)) ;
#6684 = CARTESIAN_POINT('',(32.5,-23.,-8.55662432703)) ;
#6685 = CARTESIAN_POINT('',(32.5,-24.5,-8.55662432703)) ;
#6686 = CARTESIAN_POINT('',(32.5,-26.,-11.443375673)) ;
#6687 = CARTESIAN_POINT('',(32.5,-26.,-10.)) ;
#6688 = CARTESIAN_POINT('',(32.5,-23.,-11.443375673)) ;
#6689 = CARTESIAN_POINT('',(32.5,-24.5,-11.443375673)) ;
#6690 = CARTESIAN_POINT('',(32.5,-23.,-10.)) ;
#6691 = CARTESIAN_POINT('Origin',(35.,-26.,-7.11324865405)) ;
#6692 = CARTESIAN_POINT('',(35.,-26.,-7.11324865405)) ;
#6693 = CARTESIAN_POINT('',(35.,-23.,-7.11324865405)) ;
#6694 = CARTESIAN_POINT('',(35.,-24.5,-7.11324865405)) ;
#6695 = CARTESIAN_POINT('',(33.75,-26.,-7.83493649054)) ;
#6696 = CARTESIAN_POINT('',(33.75,-23.,-7.83493649054)) ;
#6697 = CARTESIAN_POINT('Origin',(32.5,-26.,-11.443375673)) ;
#6698 = CARTESIAN_POINT('',(35.,-26.,-12.8867513459)) ;
#6699 = CARTESIAN_POINT('',(33.75,-26.,-12.1650635095)) ;
#6700 = CARTESIAN_POINT('',(35.,-23.,-12.8867513459)) ;
#6701 = CARTESIAN_POINT('',(35.,-24.5,-12.8867513459)) ;
#6702 = CARTESIAN_POINT('',(33.75,-23.,-12.1650635095)) ;
#6703 = CARTESIAN_POINT('Origin',(-35.,-23.,10.)) ;
#6704 = CARTESIAN_POINT('',(37.5,-23.,-11.443375673)) ;
#6705 = CARTESIAN_POINT('',(36.25,-23.,-12.1650635095)) ;
#6706 = CARTESIAN_POINT('',(37.5,-23.,-8.55662432703)) ;
#6707 = CARTESIAN_POINT('',(37.5,-23.,-10.)) ;
#6708 = CARTESIAN_POINT('',(36.25,-23.,-7.83493649054)) ;
#6709 = CARTESIAN_POINT('Origin',(37.5,-26.,-8.55662432703)) ;
#6710 = CARTESIAN_POINT('',(37.5,-26.,-8.55662432703)) ;
#6711 = CARTESIAN_POINT('',(37.5,-24.5,-8.55662432703)) ;
#6712 = CARTESIAN_POINT('',(36.25,-26.,-7.83493649054)) ;
#6713 = CARTESIAN_POINT('Origin',(35.,-26.,-12.8867513459)) ;
#6714 = CARTESIAN_POINT('',(37.5,-26.,-11.443375673)) ;
#6715 = CARTESIAN_POINT('',(36.25,-26.,-12.1650635095)) ;
#6716 = CARTESIAN_POINT('',(37.5,-24.5,-11.443375673)) ;
#6717 = CARTESIAN_POINT('Origin',(37.5,-26.,-11.443375673)) ;
#6718 = CARTESIAN_POINT('',(37.5,-26.,-10.)) ;
#6719 = CARTESIAN_POINT('Origin',(-35.,-26.,10.)) ;
#6720 = CARTESIAN_POINT('',(32.8905276301,-26.,-6.13863672768)) ;
#6721 = CARTESIAN_POINT('Origin',(35.,-26.,-10.)) ;
#6722 = CARTESIAN_POINT('Origin',(-35.,-20.,5.)) ;
#6723 = CARTESIAN_POINT('',(32.602872307,-20.,-5.61208719055)) ;
#6724 = CARTESIAN_POINT('Origin',(35.,-20.,-10.)) ;
#6725 = CARTESIAN_POINT('',(33.4418669995,-20.,-7.14785667386)) ;
#6726 = CARTESIAN_POINT('Origin',(35.,-20.,-10.)) ;
#6727 = CARTESIAN_POINT('Origin',(-35.,40.,7.5)) ;
#6728 = CARTESIAN_POINT('',(33.8014361535,40.,-7.80604359527)) ;
#6729 = CARTESIAN_POINT('Origin',(35.,40.,-10.)) ;
#6730 = CARTESIAN_POINT('Origin',(35.,-25.4,-10.)) ;
#6731 = CARTESIAN_POINT('',(32.602872307,-25.4,-5.61208719055)) ;
#6732 = CARTESIAN_POINT('Origin',(32.8905276301415,-25.4,-6.13863672768236)) ;
#6733 = CARTESIAN_POINT('Origin',(35.,-25.4,-10.)) ;
#6734 = CARTESIAN_POINT('Origin',(35.,7.,-10.)) ;
#6735 = CARTESIAN_POINT('',(32.602872306979,7.,-5.61208719054814)) ;
#6736 = CARTESIAN_POINT('Origin',(35.,-19.75,-10.)) ;
#6737 = CARTESIAN_POINT('',(33.5617233842,-19.75,-7.36725231433)) ;
#6738 = CARTESIAN_POINT('Origin',(33.4418669995363,-19.75,-7.14785667385629)) ;
#6739 = CARTESIAN_POINT('Origin',(35.,-19.75,-10.)) ;
#6740 = CARTESIAN_POINT('Origin',(35.,7.,-10.)) ;
#6741 = CARTESIAN_POINT('',(33.5617233842,39.5,-7.36725231433)) ;
#6742 = CARTESIAN_POINT('',(33.5617233841874,7.,-7.36725231432888)) ;
#6743 = CARTESIAN_POINT('Origin',(35.,39.5,-10.)) ;
#6744 = CARTESIAN_POINT('Origin',(35.,40.,-10.)) ;
#6745 = CARTESIAN_POINT('',(33.8014361534895,40.,-7.80604359527407)) ;
#6746 = CARTESIAN_POINT('',(0.,0.,0.)) ;
#6747 = CARTESIAN_POINT('',(0.,0.,0.)) ;
#6748 = CARTESIAN_POINT('',(0.,0.,0.)) ;
#6749 = CARTESIAN_POINT('',(0.,0.,0.)) ;
#6750 = CARTESIAN_POINT('',(0.,0.,0.)) ;
#6751 = CARTESIAN_POINT('',(0.,0.,0.)) ;
#6752 = CARTESIAN_POINT('',(0.,0.,0.)) ;
#6753 = CARTESIAN_POINT('',(0.,0.,0.)) ;
#6754 = CARTESIAN_POINT('',(0.,0.,0.)) ;
#6755 = CARTESIAN_POINT('',(0.,0.,0.)) ;
#6756 = UNCERTAINTY_MEASURE_WITH_UNIT(LENGTH_MEASURE(0.01),#6780,
'DISTANCE_ACCURACY_VALUE',
'Maximum model space distance between geometric entities at asserted c
onnectivities') ;
#6757 = UNCERTAINTY_MEASURE_WITH_UNIT(LENGTH_MEASURE(0.01),#6780,
'DISTANCE_ACCURACY_VALUE',
'Maximum model space distance between geometric entities at asserted c
onnectivities') ;
#6758 = UNCERTAINTY_MEASURE_WITH_UNIT(LENGTH_MEASURE(0.01),#6780,
'DISTANCE_ACCURACY_VALUE',
'Maximum model space distance between geometric entities at asserted c
onnectivities') ;
#6759 = UNCERTAINTY_MEASURE_WITH_UNIT(LENGTH_MEASURE(0.01),#6780,
'DISTANCE_ACCURACY_VALUE',
'Maximum model space distance between geometric entities at asserted c
onnectivities') ;
#6760 = UNCERTAINTY_MEASURE_WITH_UNIT(LENGTH_MEASURE(0.01),#6780,
'DISTANCE_ACCURACY_VALUE',
'Maximum model space distance between geometric entities at asserted c
onnectivities') ;
#6761 = UNCERTAINTY_MEASURE_WITH_UNIT(LENGTH_MEASURE(0.01),#6780,
'DISTANCE_ACCURACY_VALUE',
'Maximum model space distance between geometric entities at asserted c
onnectivities') ;
#6762 = UNCERTAINTY_MEASURE_WITH_UNIT(LENGTH_MEASURE(0.01),#6780,
'DISTANCE_ACCURACY_VALUE',
'Maximum model space distance between geometric entities at asserted c
onnectivities') ;
#6763 = UNCERTAINTY_MEASURE_WITH_UNIT(LENGTH_MEASURE(0.01),#6780,
'DISTANCE_ACCURACY_VALUE',
'Maximum model space distance between geometric entities at asserted c
onnectivities') ;
#6764 = UNCERTAINTY_MEASURE_WITH_UNIT(LENGTH_MEASURE(0.01),#6780,
'DISTANCE_ACCURACY_VALUE',
'Maximum model space distance between geometric entities at asserted c
onnectivities') ;
#6765 = UNCERTAINTY_MEASURE_WITH_UNIT(LENGTH_MEASURE(0.01),#6780,
'DISTANCE_ACCURACY_VALUE',
'Maximum model space distance between geometric entities at asserted c
onnectivities') ;
#6766 = UNCERTAINTY_MEASURE_WITH_UNIT(LENGTH_MEASURE(0.01),#6780,
'DISTANCE_ACCURACY_VALUE',
'Maximum model space distance between geometric entities at asserted c
onnectivities') ;
#6767 = UNCERTAINTY_MEASURE_WITH_UNIT(LENGTH_MEASURE(0.01),#6780,
'DISTANCE_ACCURACY_VALUE',
'Maximum model space distance between geometric entities at asserted c
onnectivities') ;
#6768 = (
GEOMETRIC_REPRESENTATION_CONTEXT(3)
GLOBAL_UNCERTAINTY_ASSIGNED_CONTEXT((#6756))
GLOBAL_UNIT_ASSIGNED_CONTEXT((#6780,#6782,#6783))
REPRESENTATION_CONTEXT('','3D')
) ;
#6769 = (
GEOMETRIC_REPRESENTATION_CONTEXT(3)
GLOBAL_UNCERTAINTY_ASSIGNED_CONTEXT((#6757))
GLOBAL_UNIT_ASSIGNED_CONTEXT((#6780,#6782,#6783))
REPRESENTATION_CONTEXT('','3D')
) ;
#6770 = (
GEOMETRIC_REPRESENTATION_CONTEXT(3)
GLOBAL_UNCERTAINTY_ASSIGNED_CONTEXT((#6758))
GLOBAL_UNIT_ASSIGNED_CONTEXT((#6780,#6782,#6783))
REPRESENTATION_CONTEXT('','3D')
) ;
#6771 = (
GEOMETRIC_REPRESENTATION_CONTEXT(3)
GLOBAL_UNCERTAINTY_ASSIGNED_CONTEXT((#6759))
GLOBAL_UNIT_ASSIGNED_CONTEXT((#6780,#6782,#6783))
REPRESENTATION_CONTEXT('','3D')
) ;
#6772 = (
GEOMETRIC_REPRESENTATION_CONTEXT(3)
GLOBAL_UNCERTAINTY_ASSIGNED_CONTEXT((#6760))
GLOBAL_UNIT_ASSIGNED_CONTEXT((#6780,#6782,#6783))
REPRESENTATION_CONTEXT('','3D')
) ;
#6773 = (
GEOMETRIC_REPRESENTATION_CONTEXT(3)
GLOBAL_UNCERTAINTY_ASSIGNED_CONTEXT((#6761))
GLOBAL_UNIT_ASSIGNED_CONTEXT((#6780,#6782,#6783))
REPRESENTATION_CONTEXT('','3D')
) ;
#6774 = (
GEOMETRIC_REPRESENTATION_CONTEXT(3)
GLOBAL_UNCERTAINTY_ASSIGNED_CONTEXT((#6762))
GLOBAL_UNIT_ASSIGNED_CONTEXT((#6780,#6782,#6783))
REPRESENTATION_CONTEXT('','3D')
) ;
#6775 = (
GEOMETRIC_REPRESENTATION_CONTEXT(3)
GLOBAL_UNCERTAINTY_ASSIGNED_CONTEXT((#6763))
GLOBAL_UNIT_ASSIGNED_CONTEXT((#6780,#6782,#6783))
REPRESENTATION_CONTEXT('','3D')
) ;
#6776 = (
GEOMETRIC_REPRESENTATION_CONTEXT(3)
GLOBAL_UNCERTAINTY_ASSIGNED_CONTEXT((#6764))
GLOBAL_UNIT_ASSIGNED_CONTEXT((#6780,#6782,#6783))
REPRESENTATION_CONTEXT('','3D')
) ;
#6777 = (
GEOMETRIC_REPRESENTATION_CONTEXT(3)
GLOBAL_UNCERTAINTY_ASSIGNED_CONTEXT((#6765))
GLOBAL_UNIT_ASSIGNED_CONTEXT((#6780,#6782,#6783))
REPRESENTATION_CONTEXT('','3D')
) ;
#6778 = (
GEOMETRIC_REPRESENTATION_CONTEXT(3)
GLOBAL_UNCERTAINTY_ASSIGNED_CONTEXT((#6766))
GLOBAL_UNIT_ASSIGNED_CONTEXT((#6780,#6782,#6783))
REPRESENTATION_CONTEXT('','3D')
) ;
#6779 = (
GEOMETRIC_REPRESENTATION_CONTEXT(3)
GLOBAL_UNCERTAINTY_ASSIGNED_CONTEXT((#6767))
GLOBAL_UNIT_ASSIGNED_CONTEXT((#6780,#6782,#6783))
REPRESENTATION_CONTEXT('','3D')
) ;
#6780 = (
LENGTH_UNIT()
NAMED_UNIT(*)
SI_UNIT(.MILLI.,.METRE.)
) ;
#6781 = (
LENGTH_UNIT()
NAMED_UNIT(*)
SI_UNIT($,.METRE.)
) ;
#6782 = (
NAMED_UNIT(*)
PLANE_ANGLE_UNIT()
SI_UNIT($,.RADIAN.)
) ;
#6783 = (
NAMED_UNIT(*)
SI_UNIT($,.STERADIAN.)
SOLID_ANGLE_UNIT()
) ;
#6784 = SHAPE_DEFINITION_REPRESENTATION(#6795,#6816) ;
#6785 = SHAPE_DEFINITION_REPRESENTATION(#6796,#6817) ;
#6786 = SHAPE_DEFINITION_REPRESENTATION(#6797,#6818) ;
#6787 = SHAPE_DEFINITION_REPRESENTATION(#6798,#6819) ;
#6788 = SHAPE_DEFINITION_REPRESENTATION(#6799,#6820) ;
#6789 = SHAPE_DEFINITION_REPRESENTATION(#6800,#6821) ;
#6790 = SHAPE_DEFINITION_REPRESENTATION(#6801,#6822) ;
#6791 = SHAPE_DEFINITION_REPRESENTATION(#6802,#6823) ;
#6792 = SHAPE_DEFINITION_REPRESENTATION(#6803,#6824) ;
#6793 = SHAPE_DEFINITION_REPRESENTATION(#6804,#6825) ;
#6794 = SHAPE_DEFINITION_REPRESENTATION(#6805,#6826) ;
#6795 = PRODUCT_DEFINITION_SHAPE('',$,#6828) ;
#6796 = PRODUCT_DEFINITION_SHAPE('',$,#6829) ;
#6797 = PRODUCT_DEFINITION_SHAPE('',$,#6830) ;
#6798 = PRODUCT_DEFINITION_SHAPE('',$,#6831) ;
#6799 = PRODUCT_DEFINITION_SHAPE('',$,#6832) ;
#6800 = PRODUCT_DEFINITION_SHAPE('',$,#6833) ;
#6801 = PRODUCT_DEFINITION_SHAPE('',$,#6834) ;
#6802 = PRODUCT_DEFINITION_SHAPE('',$,#6835) ;
#6803 = PRODUCT_DEFINITION_SHAPE('',$,#6836) ;
#6804 = PRODUCT_DEFINITION_SHAPE('',$,#6837) ;
#6805 = PRODUCT_DEFINITION_SHAPE('',$,#6838) ;
#6806 = PRODUCT_DEFINITION_SHAPE($,$,#41) ;
#6807 = PRODUCT_DEFINITION_SHAPE($,$,#42) ;
#6808 = PRODUCT_DEFINITION_SHAPE($,$,#43) ;
#6809 = PRODUCT_DEFINITION_SHAPE($,$,#44) ;
#6810 = PRODUCT_DEFINITION_SHAPE($,$,#45) ;
#6811 = PRODUCT_DEFINITION_SHAPE($,$,#46) ;
#6812 = PRODUCT_DEFINITION_SHAPE($,$,#47) ;
#6813 = PRODUCT_DEFINITION_SHAPE($,$,#48) ;
#6814 = PRODUCT_DEFINITION_SHAPE($,$,#49) ;
#6815 = PRODUCT_DEFINITION_SHAPE($,$,#50) ;
#6816 = SHAPE_REPRESENTATION('',(#4016,#4427,#4428,#4429,#4430,#4431,#4432,
#4433,#4434,#4435,#4436),#6768) ;
#6817 = SHAPE_REPRESENTATION('',(#4017),#6769) ;
#6818 = SHAPE_REPRESENTATION('',(#4192),#6770) ;
#6819 = SHAPE_REPRESENTATION('',(#4291),#6771) ;
#6820 = SHAPE_REPRESENTATION('',(#4300),#6772) ;
#6821 = SHAPE_REPRESENTATION('',(#4309),#6773) ;
#6822 = SHAPE_REPRESENTATION('',(#4318),#6774) ;
#6823 = SHAPE_REPRESENTATION('',(#4327),#6775) ;
#6824 = SHAPE_REPRESENTATION('',(#4352),#6776) ;
#6825 = SHAPE_REPRESENTATION('',(#4377),#6777) ;
#6826 = SHAPE_REPRESENTATION('',(#4402),#6778) ;
#6827 = PRODUCT_DEFINITION_CONTEXT('part definition',#6862,'design') ;
#6828 = PRODUCT_DEFINITION('MAS-636','MAS-636',#6839,#6827) ;
#6829 = PRODUCT_DEFINITION('Clamp_Body_Upper','Clamp_Body_Upper',#6840,#6827) ;
#6830 = PRODUCT_DEFINITION('Clamp_Body_Lower','Clamp_Body_Lower',#6841,#6827) ;
#6831 = PRODUCT_DEFINITION('Washer_1','Washer_1',#6842,#6827) ;
#6832 = PRODUCT_DEFINITION('Washer_2','Washer_2',#6843,#6827) ;
#6833 = PRODUCT_DEFINITION('Washer_3','Washer_3',#6844,#6827) ;
#6834 = PRODUCT_DEFINITION('Washer_4','Washer_4',#6845,#6827) ;
#6835 = PRODUCT_DEFINITION('Clamp_Bolt_1','Clamp_Bolt_1',#6846,#6827) ;
#6836 = PRODUCT_DEFINITION('Clamp_Bolt_2','Clamp_Bolt_2',#6847,#6827) ;
#6837 = PRODUCT_DEFINITION('Clamp_Bolt_3','Clamp_Bolt_3',#6848,#6827) ;
#6838 = PRODUCT_DEFINITION('Clamp_Bolt_4','Clamp_Bolt_4',#6849,#6827) ;
#6839 = PRODUCT_DEFINITION_FORMATION('',$,#6864) ;
#6840 = PRODUCT_DEFINITION_FORMATION('',$,#6865) ;
#6841 = PRODUCT_DEFINITION_FORMATION('',$,#6866) ;
#6842 = PRODUCT_DEFINITION_FORMATION('',$,#6867) ;
#6843 = PRODUCT_DEFINITION_FORMATION('',$,#6868) ;
#6844 = PRODUCT_DEFINITION_FORMATION('',$,#6869) ;
#6845 = PRODUCT_DEFINITION_FORMATION('',$,#6870) ;
#6846 = PRODUCT_DEFINITION_FORMATION('',$,#6871) ;
#6847 = PRODUCT_DEFINITION_FORMATION('',$,#6872) ;
#6848 = PRODUCT_DEFINITION_FORMATION('',$,#6873) ;
#6849 = PRODUCT_DEFINITION_FORMATION('',$,#6874) ;
#6850 = PRODUCT_RELATED_PRODUCT_CATEGORY('MAS-636','MAS-636',(#6864)) ;
#6851 = PRODUCT_RELATED_PRODUCT_CATEGORY('Clamp_Body_Upper',
'Clamp_Body_Upper',(#6865)) ;
#6852 = PRODUCT_RELATED_PRODUCT_CATEGORY('Clamp_Body_Lower',
'Clamp_Body_Lower',(#6866)) ;
#6853 = PRODUCT_RELATED_PRODUCT_CATEGORY('Washer_1','Washer_1',(#6867)) ;
#6854 = PRODUCT_RELATED_PRODUCT_CATEGORY('Washer_2','Washer_2',(#6868)) ;
#6855 = PRODUCT_RELATED_PRODUCT_CATEGORY('Washer_3','Washer_3',(#6869)) ;
#6856 = PRODUCT_RELATED_PRODUCT_CATEGORY('Washer_4','Washer_4',(#6870)) ;
#6857 = PRODUCT_RELATED_PRODUCT_CATEGORY('Clamp_Bolt_1','Clamp_Bolt_1',(#6871)) ;
#6858 = PRODUCT_RELATED_PRODUCT_CATEGORY('Clamp_Bolt_2','Clamp_Bolt_2',(#6872)) ;
#6859 = PRODUCT_RELATED_PRODUCT_CATEGORY('Clamp_Bolt_3','Clamp_Bolt_3',(#6873)) ;
#6860 = PRODUCT_RELATED_PRODUCT_CATEGORY('Clamp_Bolt_4','Clamp_Bolt_4',(#6874)) ;
#6861 = APPLICATION_PROTOCOL_DEFINITION('international standard',
'automotive_design',2009,#6862) ;
#6862 = APPLICATION_CONTEXT(
'Core Data for Automotive Mechanical Design Process') ;
#6863 = PRODUCT_CONTEXT('part definition',#6862,'mechanical') ;
#6864 = PRODUCT('MAS-636','MAS-636',$,(#6863)) ;
#6865 = PRODUCT('Clamp_Body_Upper','Clamp_Body_Upper',$,(#6863)) ;
#6866 = PRODUCT('Clamp_Body_Lower','Clamp_Body_Lower',$,(#6863)) ;
#6867 = PRODUCT('Washer_1','Washer_1',$,(#6863)) ;
#6868 = PRODUCT('Washer_2','Washer_2',$,(#6863)) ;
#6869 = PRODUCT('Washer_3','Washer_3',$,(#6863)) ;
#6870 = PRODUCT('Washer_4','Washer_4',$,(#6863)) ;
#6871 = PRODUCT('Clamp_Bolt_1','Clamp_Bolt_1',$,(#6863)) ;
#6872 = PRODUCT('Clamp_Bolt_2','Clamp_Bolt_2',$,(#6863)) ;
#6873 = PRODUCT('Clamp_Bolt_3','Clamp_Bolt_3',$,(#6863)) ;
#6874 = PRODUCT('Clamp_Bolt_4','Clamp_Bolt_4',$,(#6863)) ;
#6875 = PRESENTATION_STYLE_ASSIGNMENT((#6878)) ;
#6876 = PRESENTATION_STYLE_ASSIGNMENT((#6879)) ;
#6877 = PRESENTATION_STYLE_ASSIGNMENT((#6880)) ;
#6878 = SURFACE_STYLE_USAGE(.BOTH.,#6881) ;
#6879 = SURFACE_STYLE_USAGE(.BOTH.,#6882) ;
#6880 = SURFACE_STYLE_USAGE(.BOTH.,#6883) ;
#6881 = SURFACE_SIDE_STYLE('',(#6884)) ;
#6882 = SURFACE_SIDE_STYLE('',(#6885)) ;
#6883 = SURFACE_SIDE_STYLE('',(#6886)) ;
#6884 = SURFACE_STYLE_FILL_AREA(#6887) ;
#6885 = SURFACE_STYLE_FILL_AREA(#6888) ;
#6886 = SURFACE_STYLE_FILL_AREA(#6889) ;
#6887 = FILL_AREA_STYLE('Steel - Satin',(#6890)) ;
#6888 = FILL_AREA_STYLE('Opaque(245,245,246)',(#6891)) ;
#6889 = FILL_AREA_STYLE('Opaque(203,203,203)',(#6892)) ;
#6890 = FILL_AREA_STYLE_COLOUR('Steel - Satin',#6893) ;
#6891 = FILL_AREA_STYLE_COLOUR('Opaque(245,245,246)',#6894) ;
#6892 = FILL_AREA_STYLE_COLOUR('Opaque(203,203,203)',#6895) ;
#6893 = COLOUR_RGB('Steel - Satin', 0.09019608, 0.27058824, 0.51372549) ;
#6894 = COLOUR_RGB('Opaque(245,245,246)', 0.09019608, 0.27058824, 0.51372549) ;
#6895 = COLOUR_RGB('Opaque(203,203,203)', 0.31764706, 0.68627451, 0.89019608) ;
ENDSEC;
END-ISO-10303-21;
